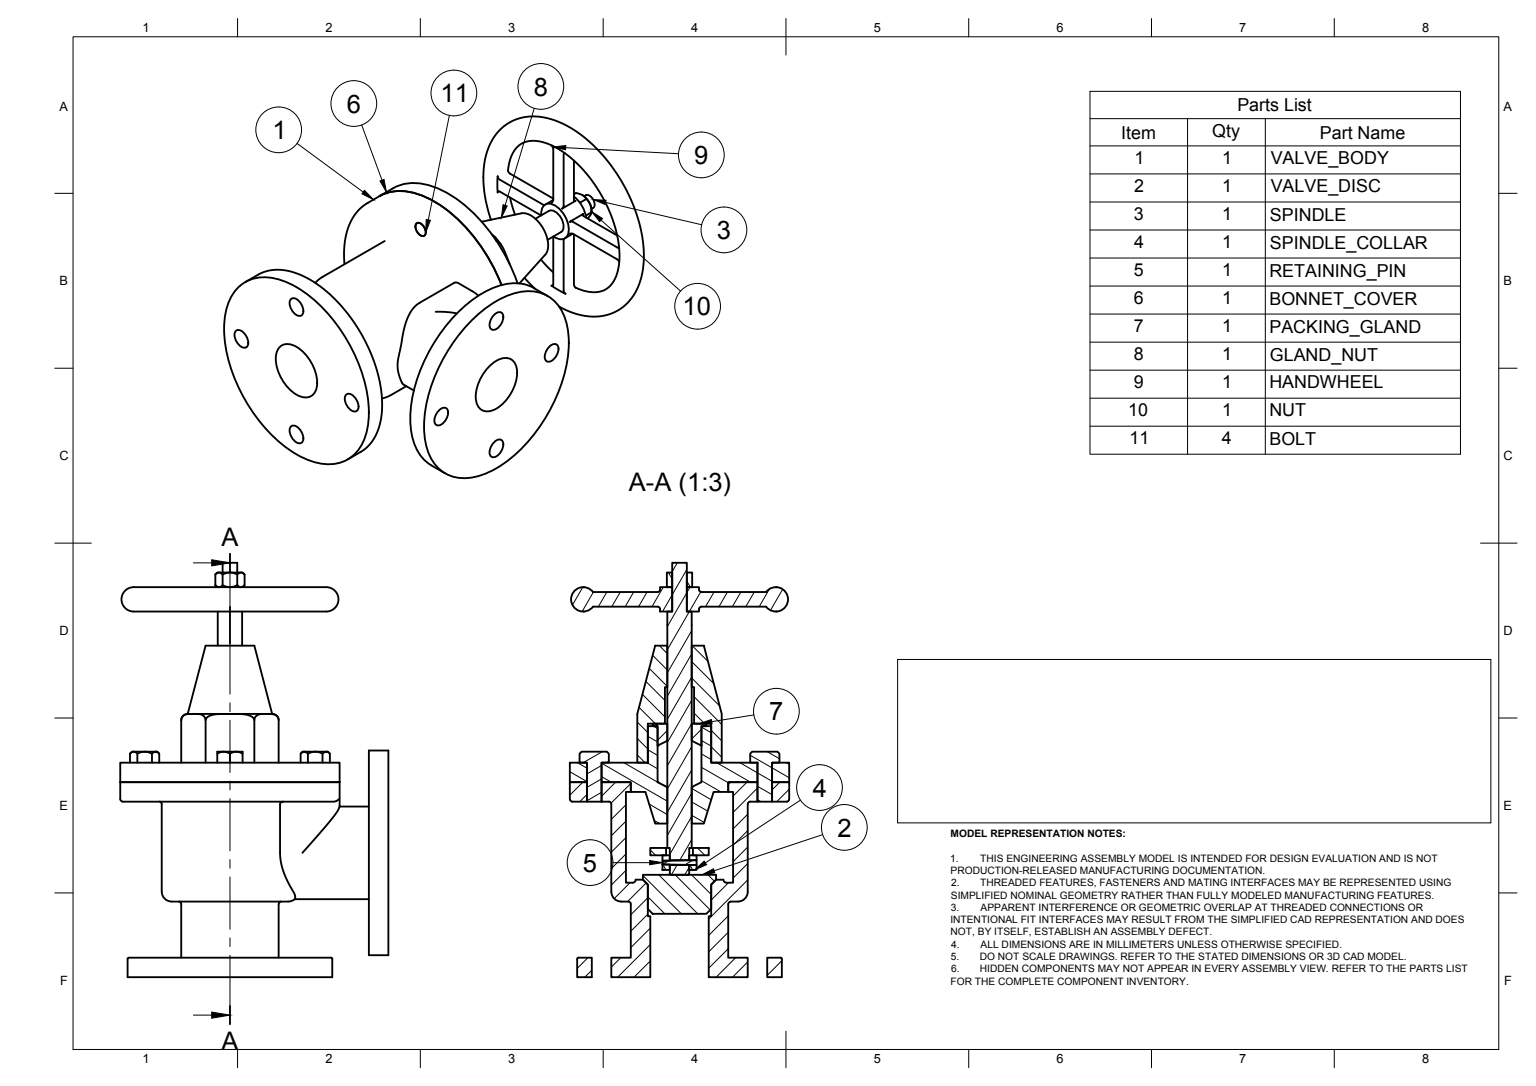
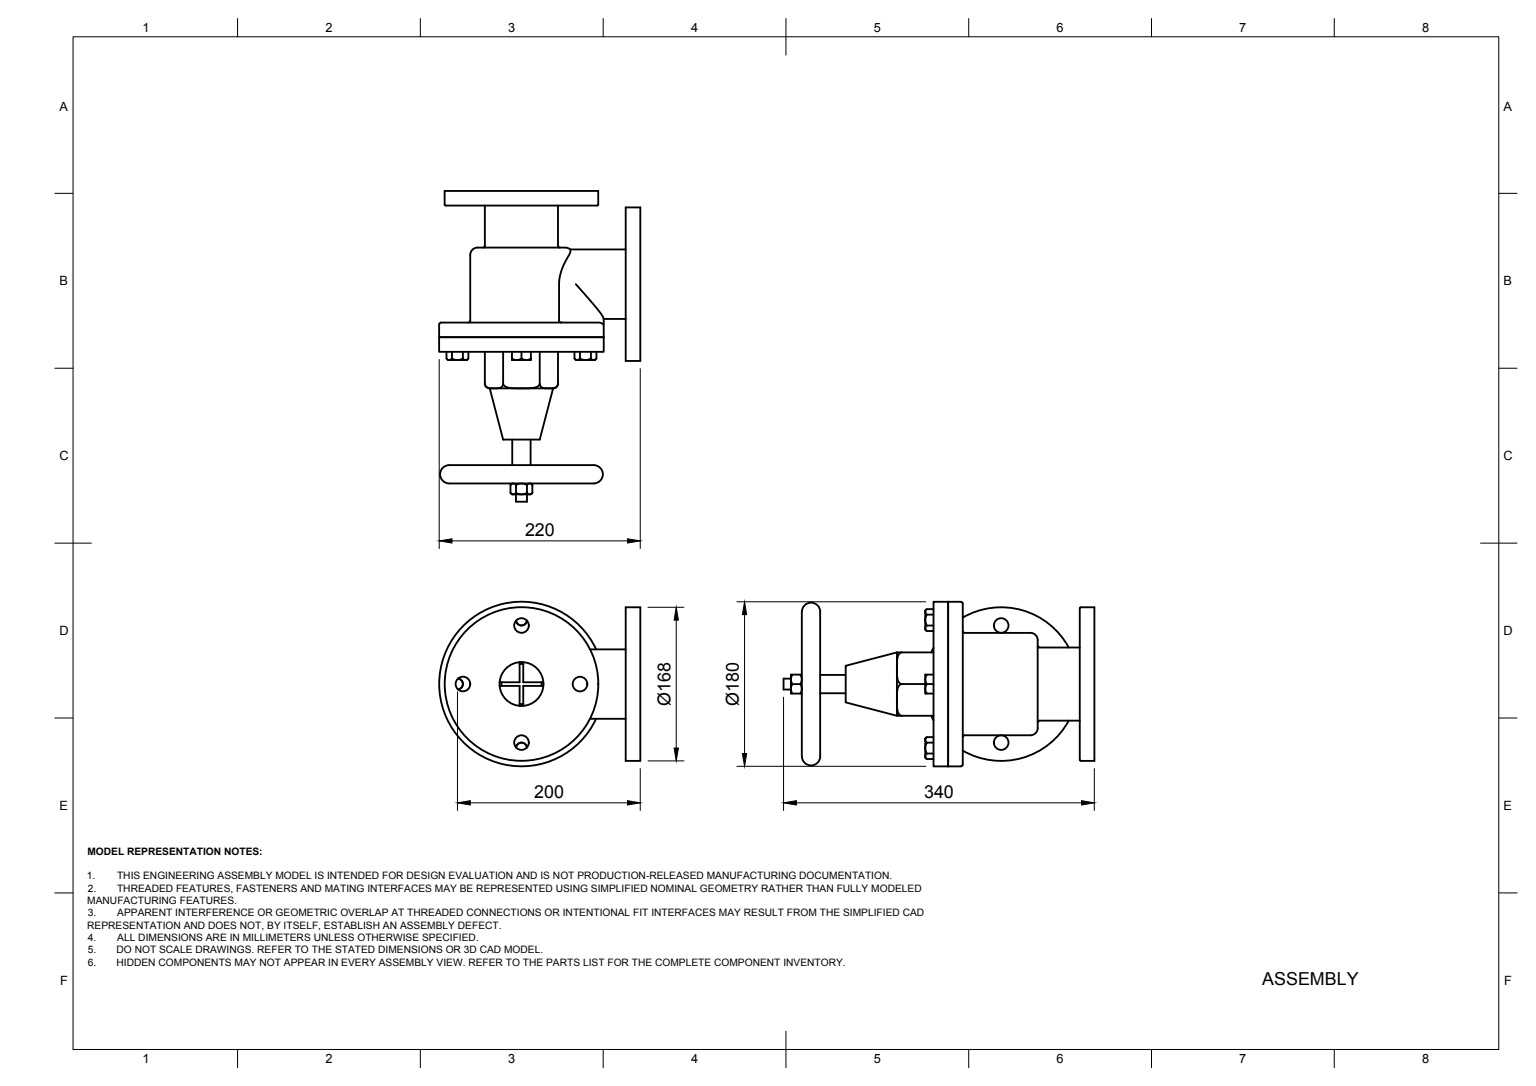
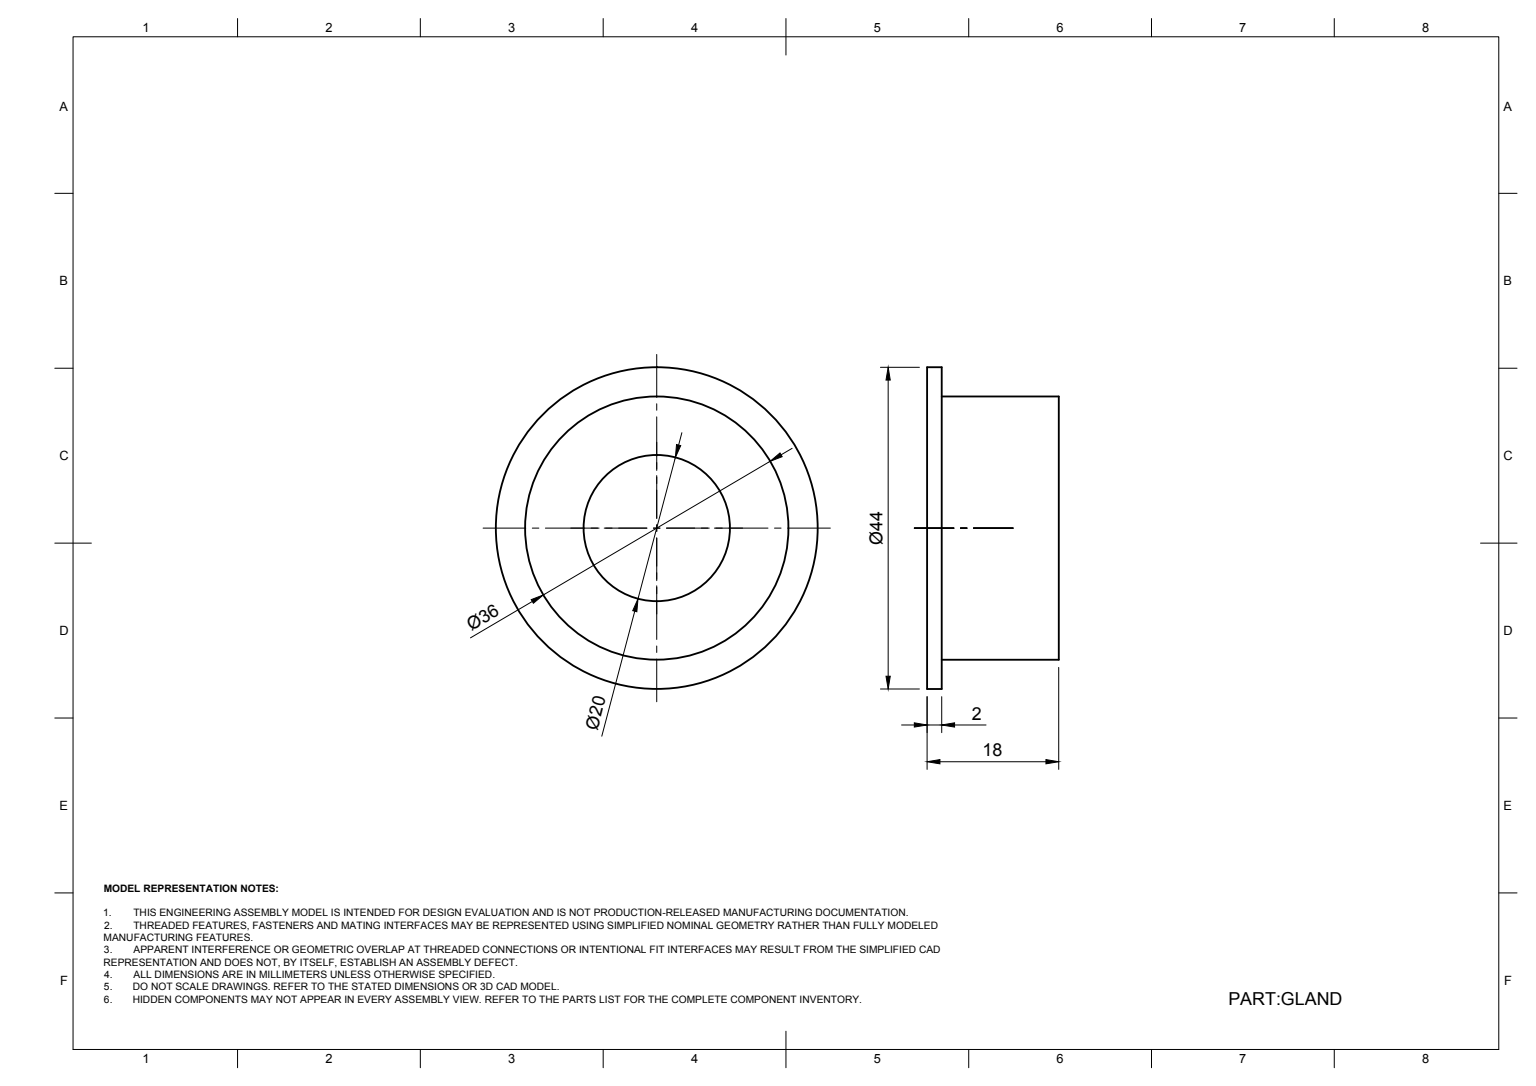
ISO-10303-21;
HEADER;
/* Generated by software containing ST-Developer
 * from STEP Tools, Inc. (www.steptools.com) 
 */

FILE_DESCRIPTION(
/* description */ (''),
/* implementation_level */ '2;1');

FILE_NAME(
/* name */ 'MAS-611',
/* time_stamp */ '2026-10-04T02:10:06-07:00',
/* author */ (''),
/* organization */ (''),
/* preprocessor_version */ 'ST-DEVELOPER v20.2',
/* originating_system */ 'Autodesk Translation Framework v15.15.0.0',
/* authorisation */ '');

FILE_SCHEMA (('AUTOMOTIVE_DESIGN { 1 0 10303 214 3 1 1 }'));
ENDSEC;

DATA;
#10=MECHANICAL_DESIGN_GEOMETRIC_PRESENTATION_REPRESENTATION('',(#141,#142,
#143,#144,#145,#146,#147,#148,#149,#150,#151),#9668);
#11=ITEM_DEFINED_TRANSFORMATION($,$,#4015,#4455);
#12=ITEM_DEFINED_TRANSFORMATION($,$,#4135,#4456);
#13=ITEM_DEFINED_TRANSFORMATION($,$,#4194,#4457);
#14=ITEM_DEFINED_TRANSFORMATION($,$,#4223,#4458);
#15=ITEM_DEFINED_TRANSFORMATION($,$,#4234,#4459);
#16=ITEM_DEFINED_TRANSFORMATION($,$,#4240,#4460);
#17=ITEM_DEFINED_TRANSFORMATION($,$,#4279,#4461);
#18=ITEM_DEFINED_TRANSFORMATION($,$,#4292,#4462);
#19=ITEM_DEFINED_TRANSFORMATION($,$,#4326,#4463);
#20=ITEM_DEFINED_TRANSFORMATION($,$,#4394,#4464);
#21=ITEM_DEFINED_TRANSFORMATION($,$,#4430,#4465);
#22=ITEM_DEFINED_TRANSFORMATION($,$,#4430,#4466);
#23=ITEM_DEFINED_TRANSFORMATION($,$,#4430,#4467);
#24=ITEM_DEFINED_TRANSFORMATION($,$,#4430,#4468);
#25=(
REPRESENTATION_RELATIONSHIP($,$,#9712,#9711)
REPRESENTATION_RELATIONSHIP_WITH_TRANSFORMATION(#11)
SHAPE_REPRESENTATION_RELATIONSHIP()
);
#26=(
REPRESENTATION_RELATIONSHIP($,$,#9713,#9711)
REPRESENTATION_RELATIONSHIP_WITH_TRANSFORMATION(#12)
SHAPE_REPRESENTATION_RELATIONSHIP()
);
#27=(
REPRESENTATION_RELATIONSHIP($,$,#9714,#9711)
REPRESENTATION_RELATIONSHIP_WITH_TRANSFORMATION(#13)
SHAPE_REPRESENTATION_RELATIONSHIP()
);
#28=(
REPRESENTATION_RELATIONSHIP($,$,#9715,#9711)
REPRESENTATION_RELATIONSHIP_WITH_TRANSFORMATION(#14)
SHAPE_REPRESENTATION_RELATIONSHIP()
);
#29=(
REPRESENTATION_RELATIONSHIP($,$,#9716,#9711)
REPRESENTATION_RELATIONSHIP_WITH_TRANSFORMATION(#15)
SHAPE_REPRESENTATION_RELATIONSHIP()
);
#30=(
REPRESENTATION_RELATIONSHIP($,$,#9717,#9711)
REPRESENTATION_RELATIONSHIP_WITH_TRANSFORMATION(#16)
SHAPE_REPRESENTATION_RELATIONSHIP()
);
#31=(
REPRESENTATION_RELATIONSHIP($,$,#9718,#9711)
REPRESENTATION_RELATIONSHIP_WITH_TRANSFORMATION(#17)
SHAPE_REPRESENTATION_RELATIONSHIP()
);
#32=(
REPRESENTATION_RELATIONSHIP($,$,#9719,#9711)
REPRESENTATION_RELATIONSHIP_WITH_TRANSFORMATION(#18)
SHAPE_REPRESENTATION_RELATIONSHIP()
);
#33=(
REPRESENTATION_RELATIONSHIP($,$,#9720,#9711)
REPRESENTATION_RELATIONSHIP_WITH_TRANSFORMATION(#19)
SHAPE_REPRESENTATION_RELATIONSHIP()
);
#34=(
REPRESENTATION_RELATIONSHIP($,$,#9721,#9711)
REPRESENTATION_RELATIONSHIP_WITH_TRANSFORMATION(#20)
SHAPE_REPRESENTATION_RELATIONSHIP()
);
#35=(
REPRESENTATION_RELATIONSHIP($,$,#9722,#9711)
REPRESENTATION_RELATIONSHIP_WITH_TRANSFORMATION(#21)
SHAPE_REPRESENTATION_RELATIONSHIP()
);
#36=(
REPRESENTATION_RELATIONSHIP($,$,#9722,#9711)
REPRESENTATION_RELATIONSHIP_WITH_TRANSFORMATION(#22)
SHAPE_REPRESENTATION_RELATIONSHIP()
);
#37=(
REPRESENTATION_RELATIONSHIP($,$,#9722,#9711)
REPRESENTATION_RELATIONSHIP_WITH_TRANSFORMATION(#23)
SHAPE_REPRESENTATION_RELATIONSHIP()
);
#38=(
REPRESENTATION_RELATIONSHIP($,$,#9722,#9711)
REPRESENTATION_RELATIONSHIP_WITH_TRANSFORMATION(#24)
SHAPE_REPRESENTATION_RELATIONSHIP()
);
#39=CONTEXT_DEPENDENT_SHAPE_REPRESENTATION(#25,#9697);
#40=CONTEXT_DEPENDENT_SHAPE_REPRESENTATION(#26,#9698);
#41=CONTEXT_DEPENDENT_SHAPE_REPRESENTATION(#27,#9699);
#42=CONTEXT_DEPENDENT_SHAPE_REPRESENTATION(#28,#9700);
#43=CONTEXT_DEPENDENT_SHAPE_REPRESENTATION(#29,#9701);
#44=CONTEXT_DEPENDENT_SHAPE_REPRESENTATION(#30,#9702);
#45=CONTEXT_DEPENDENT_SHAPE_REPRESENTATION(#31,#9703);
#46=CONTEXT_DEPENDENT_SHAPE_REPRESENTATION(#32,#9704);
#47=CONTEXT_DEPENDENT_SHAPE_REPRESENTATION(#33,#9705);
#48=CONTEXT_DEPENDENT_SHAPE_REPRESENTATION(#34,#9706);
#49=CONTEXT_DEPENDENT_SHAPE_REPRESENTATION(#35,#9707);
#50=CONTEXT_DEPENDENT_SHAPE_REPRESENTATION(#36,#9708);
#51=CONTEXT_DEPENDENT_SHAPE_REPRESENTATION(#37,#9709);
#52=CONTEXT_DEPENDENT_SHAPE_REPRESENTATION(#38,#9710);
#53=NEXT_ASSEMBLY_USAGE_OCCURRENCE('VALVE_BODY:1','VALVE_BODY:1',
'VALVE_BODY:1',#9724,#9725,'VALVE_BODY:1');
#54=NEXT_ASSEMBLY_USAGE_OCCURRENCE('VALVE_DISC:1','VALVE_DISC:1',
'VALVE_DISC:1',#9724,#9726,'VALVE_DISC:1');
#55=NEXT_ASSEMBLY_USAGE_OCCURRENCE('SPINDLE:1','SPINDLE:1','SPINDLE:1',
#9724,#9727,'SPINDLE:1');
#56=NEXT_ASSEMBLY_USAGE_OCCURRENCE('SPINDLE_COLLAR:1',
'SPINDLE_COLLAR:1','SPINDLE_COLLAR:1',#9724,#9728,'SPINDLE_COLLAR:1');
#57=NEXT_ASSEMBLY_USAGE_OCCURRENCE('RETAINING_PIN:1','RETAINING_PIN:1',
'RETAINING_PIN:1',#9724,#9729,'RETAINING_PIN:1');
#58=NEXT_ASSEMBLY_USAGE_OCCURRENCE('BONNET_COVER:1','BONNET_COVER:1',
'BONNET_COVER:1',#9724,#9730,'BONNET_COVER:1');
#59=NEXT_ASSEMBLY_USAGE_OCCURRENCE('PACKING_GLAND:1','PACKING_GLAND:1',
'PACKING_GLAND:1',#9724,#9731,'PACKING_GLAND:1');
#60=NEXT_ASSEMBLY_USAGE_OCCURRENCE('GLAND_NUT:1','GLAND_NUT:1',
'GLAND_NUT:1',#9724,#9732,'GLAND_NUT:1');
#61=NEXT_ASSEMBLY_USAGE_OCCURRENCE('HANDWHEEL:1','HANDWHEEL:1',
'HANDWHEEL:1',#9724,#9733,'HANDWHEEL:1');
#62=NEXT_ASSEMBLY_USAGE_OCCURRENCE('NUT:1','NUT:1','NUT:1',#9724,#9734,
'NUT:1');
#63=NEXT_ASSEMBLY_USAGE_OCCURRENCE('BOLT:1','BOLT:1','BOLT:1',#9724,#9735,
'BOLT:1');
#64=NEXT_ASSEMBLY_USAGE_OCCURRENCE('BOLT:2','BOLT:2','BOLT:2',#9724,#9735,
'BOLT:2');
#65=NEXT_ASSEMBLY_USAGE_OCCURRENCE('BOLT:3','BOLT:3','BOLT:3',#9724,#9735,
'BOLT:3');
#66=NEXT_ASSEMBLY_USAGE_OCCURRENCE('BOLT:4','BOLT:4','BOLT:4',#9724,#9735,
'BOLT:4');
#67=(
BOUNDED_SURFACE()
B_SPLINE_SURFACE(3,2,((#8974,#8975,#8976),(#8977,#8978,#8979),(#8980,#8981,
#8982),(#8983,#8984,#8985),(#8986,#8987,#8988),(#8989,#8990,#8991),(#8992,
#8993,#8994),(#8995,#8996,#8997),(#8998,#8999,#9000),(#9001,#9002,#9003),
(#9004,#9005,#9006),(#9007,#9008,#9009),(#9010,#9011,#9012),(#9013,#9014,
#9015),(#9016,#9017,#9018),(#9019,#9020,#9021),(#9022,#9023,#9024),(#9025,
#9026,#9027)),.UNSPECIFIED.,.F.,.F.,.F.)
B_SPLINE_SURFACE_WITH_KNOTS((4,1,1,1,1,1,1,1,1,1,1,1,1,1,1,4),(3,3),(0.0314788030428868,
0.0324522874563819,0.0334257718698771,0.0353727406968673,0.0363462251103625,
0.0373197095238576,0.0382931939373528,0.0392666783508479,0.0402401627643431,
0.0412136471778382,0.0421871315913334,0.0431606160048285,0.0441341004183236,
0.0451075848318188,0.0460810692453139,0.0470545536588091),(0.,1.),
 .UNSPECIFIED.)
GEOMETRIC_REPRESENTATION_ITEM()
RATIONAL_B_SPLINE_SURFACE(((1.,0.673965297618148,1.),(1.,0.673166296515258,
1.),(1.,0.671622878424884,1.),(1.,0.668872043360916,1.),(1.,0.6666737415125,
1.),(1.,0.665066367000124,1.),(1.,0.664191179384959,1.),(1.,0.663664801981856,
1.),(1.,0.663490402453091,1.),(1.,0.663673371681184,1.),(1.,0.664201607885415,
1.),(1.,0.66506767873011,1.),(1.,0.666279408316226,1.),(1.,0.667792932640577,
1.),(1.,0.669583017900756,1.),(1.,0.671633975311695,1.),(1.,0.673174922786531,
1.),(1.,0.673980190168732,1.)))
REPRESENTATION_ITEM('')
SURFACE()
);
#68=(
BOUNDED_SURFACE()
B_SPLINE_SURFACE(3,2,((#9028,#9029,#9030),(#9031,#9032,#9033),(#9034,#9035,
#9036),(#9037,#9038,#9039),(#9040,#9041,#9042),(#9043,#9044,#9045),(#9046,
#9047,#9048),(#9049,#9050,#9051),(#9052,#9053,#9054),(#9055,#9056,#9057),
(#9058,#9059,#9060),(#9061,#9062,#9063),(#9064,#9065,#9066),(#9067,#9068,
#9069),(#9070,#9071,#9072),(#9073,#9074,#9075),(#9076,#9077,#9078),(#9079,
#9080,#9081)),.UNSPECIFIED.,.F.,.F.,.F.)
B_SPLINE_SURFACE_WITH_KNOTS((4,1,1,1,1,1,1,1,1,1,1,1,1,1,1,4),(3,3),(0.0306904631349172,
0.0316643361466102,0.0326382091583032,0.0336120821699963,0.0345859551816893,
0.0355598281933823,0.0365337012050753,0.0375075742167683,0.0384814472284614,
0.0394553202401544,0.0404291932518474,0.0414030662635404,0.0423769392752334,
0.0433508122869265,0.0443246852986195,0.0462724313220055),(0.,1.),
 .UNSPECIFIED.)
GEOMETRIC_REPRESENTATION_ITEM()
RATIONAL_B_SPLINE_SURFACE(((1.,0.673964349039136,1.),(1.,0.673168502978567,
1.),(1.,0.671643925861953,1.),(1.,0.669562296886318,1.),(1.,0.667767007356651,
1.),(1.,0.666266776870979,1.),(1.,0.665071978074277,1.),(1.,0.664194007330874,
1.),(1.,0.663665542131989,1.),(1.,0.663490103902602,1.),(1.,0.663673710164509,
1.),(1.,0.664205908065376,1.),(1.,0.665074561266886,1.),(1.,0.666270920547672,
1.),(1.,0.667799410011383,1.),(1.,0.670197938500333,1.),(1.,0.672375755500364,
1.),(1.,0.673978916833767,1.)))
REPRESENTATION_ITEM('')
SURFACE()
);
#69=(
BOUNDED_SURFACE()
B_SPLINE_SURFACE(3,2,((#9082,#9083,#9084),(#9085,#9086,#9087),(#9088,#9089,
#9090),(#9091,#9092,#9093),(#9094,#9095,#9096),(#9097,#9098,#9099),(#9100,
#9101,#9102),(#9103,#9104,#9105),(#9106,#9107,#9108),(#9109,#9110,#9111),
(#9112,#9113,#9114),(#9115,#9116,#9117),(#9118,#9119,#9120),(#9121,#9122,
#9123),(#9124,#9125,#9126),(#9127,#9128,#9129),(#9130,#9131,#9132),(#9133,
#9134,#9135)),.UNSPECIFIED.,.F.,.F.,.F.)
B_SPLINE_SURFACE_WITH_KNOTS((4,1,1,1,1,1,1,1,1,1,1,1,1,1,1,4),(3,3),(0.0305897871911959,
0.0315636944986189,0.0325376018060419,0.0335115091134649,0.0344854164208879,
0.0354593237283109,0.0364332310357338,0.0374071383431568,0.0383810456505798,
0.0393549529580028,0.0403288602654258,0.0413027675728487,0.0422766748802717,
0.0432505821876947,0.0442244894951177,0.0461723041099637),(0.,1.),
 .UNSPECIFIED.)
GEOMETRIC_REPRESENTATION_ITEM()
RATIONAL_B_SPLINE_SURFACE(((1.,0.673964296834234,1.),(1.,0.673168609933157,
1.),(1.,0.671645019887839,1.),(1.,0.669565127304379,1.),(1.,0.667766560497273,
1.),(1.,0.666266474426915,1.),(1.,0.66507215658795,1.),(1.,0.664195156886529,
1.),(1.,0.663665573830476,1.),(1.,0.663490167959275,1.),(1.,0.663673406028792,
1.),(1.,0.664206149646574,1.),(1.,0.665075135400244,1.),(1.,0.666270395103817,
1.),(1.,0.667798233506142,1.),(1.,0.670199686629813,1.),(1.,0.672377030394903,
1.),(1.,0.673978715902987,1.)))
REPRESENTATION_ITEM('')
SURFACE()
);
#70=(
BOUNDED_SURFACE()
B_SPLINE_SURFACE(3,2,((#9136,#9137,#9138),(#9139,#9140,#9141),(#9142,#9143,
#9144),(#9145,#9146,#9147),(#9148,#9149,#9150),(#9151,#9152,#9153),(#9154,
#9155,#9156),(#9157,#9158,#9159),(#9160,#9161,#9162),(#9163,#9164,#9165),
(#9166,#9167,#9168),(#9169,#9170,#9171),(#9172,#9173,#9174),(#9175,#9176,
#9177),(#9178,#9179,#9180),(#9181,#9182,#9183),(#9184,#9185,#9186),(#9187,
#9188,#9189)),.UNSPECIFIED.,.F.,.F.,.F.)
B_SPLINE_SURFACE_WITH_KNOTS((4,1,1,1,1,1,1,1,1,1,1,1,1,1,1,4),(3,3),(0.0315789108977846,
0.0325523529389518,0.0335257949801189,0.0354726790624532,0.0364461211036204,
0.0374195631447876,0.0383930051859547,0.0393664472271219,0.040339889268289,
0.0413133313094562,0.0422867733506233,0.0432602153917905,0.0442336574329576,
0.0452070994741248,0.046180541515292,0.0471539835564591),(0.,1.),
 .UNSPECIFIED.)
GEOMETRIC_REPRESENTATION_ITEM()
RATIONAL_B_SPLINE_SURFACE(((1.,0.673965492863365,1.),(1.,0.673165826863236,
1.),(1.,0.671620469526443,1.),(1.,0.668874652098692,1.),(1.,0.666674941728974,
1.),(1.,0.665065162761098,1.),(1.,0.664191461531519,1.),(1.,0.663664604196809,
1.),(1.,0.663490522562251,1.),(1.,0.663673087023803,1.),(1.,0.664200791428412,
1.),(1.,0.665067176842279,1.),(1.,0.666279817333014,1.),(1.,0.667791010794828,
1.),(1.,0.669580698382089,1.),(1.,0.671631849583161,1.),(1.,0.673175667819509,
1.),(1.,0.673979886421463,1.)))
REPRESENTATION_ITEM('')
SURFACE()
);
#71=(
BOUNDED_SURFACE()
B_SPLINE_SURFACE(3,2,((#9190,#9191,#9192),(#9193,#9194,#9195),(#9196,#9197,
#9198),(#9199,#9200,#9201),(#9202,#9203,#9204),(#9205,#9206,#9207),(#9208,
#9209,#9210),(#9211,#9212,#9213),(#9214,#9215,#9216),(#9217,#9218,#9219),
(#9220,#9221,#9222),(#9223,#9224,#9225),(#9226,#9227,#9228),(#9229,#9230,
#9231),(#9232,#9233,#9234),(#9235,#9236,#9237)),.UNSPECIFIED.,.F.,.F.,.F.)
B_SPLINE_SURFACE_WITH_KNOTS((4,1,1,1,1,1,1,1,1,1,1,1,1,4),(3,3),(0.03215789731342,
0.0331313751868945,0.034104853060369,0.0350783309338435,0.0360518088073179,
0.0370252866807924,0.0379987645542669,0.0389722424277414,0.0399457203012159,
0.0418926760481649,0.0438396317951138,0.0457865875420628,0.0467600654155373,
0.0477335432890118),(-8.08454907084105E-6,1.),.UNSPECIFIED.)
GEOMETRIC_REPRESENTATION_ITEM()
RATIONAL_B_SPLINE_SURFACE(((1.00000527170182,0.673964387359616,1.),(1.00000528471687,
0.673159453411099,1.),(1.00000530961685,0.671619480347489,1.),(1.00000534275063,
0.669570276226346,1.),(1.00000537166522,0.66778201413489,1.),(1.00000539609675,
0.666271012581043,1.),(1.00000541568478,0.665059564372101,1.),(1.00000542974255,
0.664190142086893,1.),(1.000005438313,0.663660090710924,1.),(1.00000544199604,
0.663432308407853,1.),(1.00000543253772,0.664017270646154,1.),(1.00000539844928,
0.666125517336438,1.),(1.00000535391695,0.668879680311451,1.),(1.00000530941503,
0.671631962440139,1.),(1.00000528444356,0.673176357213759,1.),(1.00000527151599,
0.673975880021096,1.)))
REPRESENTATION_ITEM('')
SURFACE()
);
#72=(
BOUNDED_SURFACE()
B_SPLINE_SURFACE(3,2,((#9238,#9239,#9240),(#9241,#9242,#9243),(#9244,#9245,
#9246),(#9247,#9248,#9249),(#9250,#9251,#9252),(#9253,#9254,#9255),(#9256,
#9257,#9258),(#9259,#9260,#9261),(#9262,#9263,#9264),(#9265,#9266,#9267),
(#9268,#9269,#9270),(#9271,#9272,#9273),(#9274,#9275,#9276),(#9277,#9278,
#9279),(#9280,#9281,#9282),(#9283,#9284,#9285)),.UNSPECIFIED.,.F.,.F.,.F.)
B_SPLINE_SURFACE_WITH_KNOTS((4,1,1,1,1,1,1,1,1,1,1,1,1,4),(3,3),(0.0300049518513901,
0.031953018177045,0.0329270513398724,0.0339010845026998,0.0348751176655272,
0.0358491508283546,0.036823183991182,0.0377972171540094,0.0387712503168368,
0.0397452834796642,0.041693349805319,0.0426673829681464,0.0436414161309738,
0.0455894824566286),(0.,1.),.UNSPECIFIED.)
GEOMETRIC_REPRESENTATION_ITEM()
RATIONAL_B_SPLINE_SURFACE(((1.,0.673964297815332,1.),(1.,0.672372618458235,
1.),(1.,0.670191181394266,1.),(1.,0.667767841290405,1.),(1.,0.666265347639804,
1.),(1.,0.665072121147338,1.),(1.,0.664201207028703,1.),(1.,0.663666605647771,
1.),(1.,0.663490715236844,1.),(1.,0.663670119784287,1.),(1.,0.664385152559804,
1.),(1.,0.665767066134064,1.),(1.,0.66778345083312,1.),(1.,0.670206332337341,
1.),(1.,0.672382580991143,1.),(1.,0.673977852527306,1.)))
REPRESENTATION_ITEM('')
SURFACE()
);
#73=(
BOUNDED_SURFACE()
B_SPLINE_SURFACE(3,2,((#9286,#9287,#9288),(#9289,#9290,#9291),(#9292,#9293,
#9294),(#9295,#9296,#9297),(#9298,#9299,#9300),(#9301,#9302,#9303),(#9304,
#9305,#9306),(#9307,#9308,#9309),(#9310,#9311,#9312),(#9313,#9314,#9315),
(#9316,#9317,#9318),(#9319,#9320,#9321),(#9322,#9323,#9324),(#9325,#9326,
#9327),(#9328,#9329,#9330),(#9331,#9332,#9333),(#9334,#9335,#9336),(#9337,
#9338,#9339),(#9340,#9341,#9342)),.UNSPECIFIED.,.F.,.F.,.F.)
B_SPLINE_SURFACE_WITH_KNOTS((4,1,1,1,1,1,1,1,1,1,1,1,1,1,1,1,4),(3,3),(0.0317649381765832,
0.0327383392942574,0.0337117404119316,0.0346851415296058,0.03565854264728,
0.0366319437649542,0.0376053448826284,0.0385787460003026,0.0395521471179768,
0.040525548235651,0.0414989493533253,0.0424723504709995,0.0434457515886737,
0.0444191527063479,0.0453925538240221,0.0463659549416963,0.0473393560593705),
(0.,1.),.UNSPECIFIED.)
GEOMETRIC_REPRESENTATION_ITEM()
RATIONAL_B_SPLINE_SURFACE(((1.,0.673965909365134,1.),(1.,0.673164818236142,
1.),(1.,0.671618061862569,1.),(1.,0.669564320284071,1.),(1.,0.66777759511695,
1.),(1.,0.666273471258361,1.),(1.,0.665063410818969,1.),(1.,0.664191967652661,
1.),(1.,0.663664156821065,1.),(1.,0.663490769293391,1.),(1.,0.663672536496092,
1.),(1.,0.664199292987571,1.),(1.,0.665067031441957,1.),(1.,0.666280071948857,
1.),(1.,0.66778774864528,1.),(1.,0.669576760671401,1.),(1.,0.671629936935393,
1.),(1.,0.673176919539912,1.),(1.,0.673979374441674,1.)))
REPRESENTATION_ITEM('')
SURFACE()
);
#74=(
BOUNDED_SURFACE()
B_SPLINE_SURFACE(3,2,((#9343,#9344,#9345),(#9346,#9347,#9348),(#9349,#9350,
#9351),(#9352,#9353,#9354),(#9355,#9356,#9357),(#9358,#9359,#9360),(#9361,
#9362,#9363),(#9364,#9365,#9366),(#9367,#9368,#9369),(#9370,#9371,#9372),
(#9373,#9374,#9375),(#9376,#9377,#9378),(#9379,#9380,#9381),(#9382,#9383,
#9384),(#9385,#9386,#9387),(#9388,#9389,#9390),(#9391,#9392,#9393)),
 .UNSPECIFIED.,.F.,.F.,.F.)
B_SPLINE_SURFACE_WITH_KNOTS((4,1,1,1,1,1,1,1,1,1,1,1,1,1,4),(3,3),(0.0304023584176636,
0.0313763197495467,0.0323502810814299,0.0333242424133131,0.0342982037451962,
0.0352721650770794,0.0362461264089626,0.0372200877408457,0.0381940490727289,
0.0391680104046121,0.0401419717364953,0.0420898944002616,0.0430638557321448,
0.0440378170640279,0.0459857397277943),(0.,1.),.UNSPECIFIED.)
GEOMETRIC_REPRESENTATION_ITEM()
RATIONAL_B_SPLINE_SURFACE(((1.,0.673964240667089,1.),(1.,0.673168704865034,
1.),(1.,0.671646043506943,1.),(1.,0.669571927360062,1.),(1.,0.667765968900773,
1.),(1.,0.666266091842261,1.),(1.,0.665072243840693,1.),(1.,0.664197515743925,
1.),(1.,0.663665655019745,1.),(1.,0.663490373557035,1.),(1.,0.663672476132646,
1.),(1.,0.664385168150455,1.),(1.,0.665762507320331,1.),(1.,0.667794613454947,
1.),(1.,0.670202685638588,1.),(1.,0.672379152055614,1.),(1.,0.6739783830491,
1.)))
REPRESENTATION_ITEM('')
SURFACE()
);
#75=(
BOUNDED_CURVE()
B_SPLINE_CURVE(2,(#6291,#6292,#6293),.UNSPECIFIED.,.F.,.F.)
B_SPLINE_CURVE_WITH_KNOTS((3,3),(-0.968089558975317,-0.208236182755166),
 .UNSPECIFIED.)
CURVE()
GEOMETRIC_REPRESENTATION_ITEM()
RATIONAL_B_SPLINE_CURVE((1.03202593839996,1.02394290093172,1.00881846372195))
REPRESENTATION_ITEM('')
);
#76=(
BOUNDED_CURVE()
B_SPLINE_CURVE(2,(#6302,#6303,#6304),.UNSPECIFIED.,.F.,.F.)
B_SPLINE_CURVE_WITH_KNOTS((3,3),(-3.47246065490362,-2.71260727868867),
 .UNSPECIFIED.)
CURVE()
GEOMETRIC_REPRESENTATION_ITEM()
RATIONAL_B_SPLINE_CURVE((1.00881846372215,1.02394290093178,1.03202593839996))
REPRESENTATION_ITEM('')
);
#77=(
BOUNDED_CURVE()
B_SPLINE_CURVE(2,(#6312,#6313,#6314),.UNSPECIFIED.,.F.,.F.)
B_SPLINE_CURVE_WITH_KNOTS((3,3),(-3.47246065490362,-2.71260727868867),
 .UNSPECIFIED.)
CURVE()
GEOMETRIC_REPRESENTATION_ITEM()
RATIONAL_B_SPLINE_CURVE((1.00881846372215,1.02394290093178,1.03202593839996))
REPRESENTATION_ITEM('')
);
#78=(
BOUNDED_CURVE()
B_SPLINE_CURVE(2,(#6321,#6322,#6323),.UNSPECIFIED.,.F.,.F.)
B_SPLINE_CURVE_WITH_KNOTS((3,3),(-0.968089558975317,-0.208236182755166),
 .UNSPECIFIED.)
CURVE()
GEOMETRIC_REPRESENTATION_ITEM()
RATIONAL_B_SPLINE_CURVE((1.03202593839996,1.02394290093172,1.00881846372195))
REPRESENTATION_ITEM('')
);
#79=(
BOUNDED_CURVE()
B_SPLINE_CURVE(2,(#6399,#6400,#6401),.UNSPECIFIED.,.F.,.F.)
B_SPLINE_CURVE_WITH_KNOTS((3,3),(-3.47246065490413,-2.71260727868925),
 .UNSPECIFIED.)
CURVE()
GEOMETRIC_REPRESENTATION_ITEM()
RATIONAL_B_SPLINE_CURVE((1.00881846372252,1.0239429009328,1.03202593840134))
REPRESENTATION_ITEM('')
);
#80=(
BOUNDED_CURVE()
B_SPLINE_CURVE(2,(#6406,#6407,#6408),.UNSPECIFIED.,.F.,.F.)
B_SPLINE_CURVE_WITH_KNOTS((3,3),(-0.968089559028266,-0.20823618276597),
 .UNSPECIFIED.)
CURVE()
GEOMETRIC_REPRESENTATION_ITEM()
RATIONAL_B_SPLINE_CURVE((1.03202593842995,1.02394290095447,1.00881846373032))
REPRESENTATION_ITEM('')
);
#81=(
BOUNDED_CURVE()
B_SPLINE_CURVE(2,(#6413,#6414,#6415),.UNSPECIFIED.,.F.,.F.)
B_SPLINE_CURVE_WITH_KNOTS((3,3),(-3.47246065490413,-2.71260727868925),
 .UNSPECIFIED.)
CURVE()
GEOMETRIC_REPRESENTATION_ITEM()
RATIONAL_B_SPLINE_CURVE((1.00881846372251,1.0239429009328,1.03202593840134))
REPRESENTATION_ITEM('')
);
#82=(
BOUNDED_CURVE()
B_SPLINE_CURVE(2,(#6420,#6421,#6422),.UNSPECIFIED.,.F.,.F.)
B_SPLINE_CURVE_WITH_KNOTS((3,3),(-0.968089559028514,-0.208236182766157),
 .UNSPECIFIED.)
CURVE()
GEOMETRIC_REPRESENTATION_ITEM()
RATIONAL_B_SPLINE_CURVE((1.03202593842948,1.02394290095412,1.0088184637302))
REPRESENTATION_ITEM('')
);
#83=(
BOUNDED_CURVE()
B_SPLINE_CURVE(2,(#9398,#9399,#9400),.UNSPECIFIED.,.F.,.F.)
B_SPLINE_CURVE_WITH_KNOTS((3,3),(1.40089977676118,2.46618168478736),
 .UNSPECIFIED.)
CURVE()
GEOMETRIC_REPRESENTATION_ITEM()
RATIONAL_B_SPLINE_CURVE((1.50876305611317,1.62546628464682,1.62546628464682))
REPRESENTATION_ITEM('')
);
#84=(
BOUNDED_CURVE()
B_SPLINE_CURVE(2,(#9404,#9405,#9406),.UNSPECIFIED.,.F.,.F.)
B_SPLINE_CURVE_WITH_KNOTS((3,3),(2.46617097132528,3.53145008162195),
 .UNSPECIFIED.)
CURVE()
GEOMETRIC_REPRESENTATION_ITEM()
RATIONAL_B_SPLINE_CURVE((1.6254627916221,1.6254627916221,1.50875981387633))
REPRESENTATION_ITEM('')
);
#85=(
BOUNDED_CURVE()
B_SPLINE_CURVE(2,(#9408,#9409,#9410),.UNSPECIFIED.,.F.,.F.)
B_SPLINE_CURVE_WITH_KNOTS((3,3),(1.40089186102861,2.46617097132528),
 .UNSPECIFIED.)
CURVE()
GEOMETRIC_REPRESENTATION_ITEM()
RATIONAL_B_SPLINE_CURVE((1.50875981387633,1.6254627916221,1.6254627916221))
REPRESENTATION_ITEM('')
);
#86=(
BOUNDED_CURVE()
B_SPLINE_CURVE(2,(#9413,#9414,#9415),.UNSPECIFIED.,.F.,.F.)
B_SPLINE_CURVE_WITH_KNOTS((3,3),(2.46617097132528,3.5314500816219),
 .UNSPECIFIED.)
CURVE()
GEOMETRIC_REPRESENTATION_ITEM()
RATIONAL_B_SPLINE_CURVE((1.6254627916221,1.6254627916221,1.50875981387634))
REPRESENTATION_ITEM('')
);
#87=(
BOUNDED_CURVE()
B_SPLINE_CURVE(2,(#9419,#9420,#9421),.UNSPECIFIED.,.F.,.F.)
B_SPLINE_CURVE_WITH_KNOTS((3,3),(1.40089977676118,2.46618168478736),
 .UNSPECIFIED.)
CURVE()
GEOMETRIC_REPRESENTATION_ITEM()
RATIONAL_B_SPLINE_CURVE((1.50876305611317,1.62546628464682,1.62546628464682))
REPRESENTATION_ITEM('')
);
#88=(
BOUNDED_CURVE()
B_SPLINE_CURVE(2,(#9425,#9426,#9427),.UNSPECIFIED.,.F.,.F.)
B_SPLINE_CURVE_WITH_KNOTS((3,3),(2.46617097132528,3.53145008162194),
 .UNSPECIFIED.)
CURVE()
GEOMETRIC_REPRESENTATION_ITEM()
RATIONAL_B_SPLINE_CURVE((1.6254627916221,1.6254627916221,1.50875981387633))
REPRESENTATION_ITEM('')
);
#89=(
BOUNDED_CURVE()
B_SPLINE_CURVE(2,(#9428,#9429,#9430),.UNSPECIFIED.,.F.,.F.)
B_SPLINE_CURVE_WITH_KNOTS((3,3),(1.40089186102861,2.46617097132528),
 .UNSPECIFIED.)
CURVE()
GEOMETRIC_REPRESENTATION_ITEM()
RATIONAL_B_SPLINE_CURVE((1.50875981387633,1.6254627916221,1.6254627916221))
REPRESENTATION_ITEM('')
);
#90=(
BOUNDED_CURVE()
B_SPLINE_CURVE(2,(#9431,#9432,#9433),.UNSPECIFIED.,.F.,.F.)
B_SPLINE_CURVE_WITH_KNOTS((3,3),(2.46617097132528,3.53145008162195),
 .UNSPECIFIED.)
CURVE()
GEOMETRIC_REPRESENTATION_ITEM()
RATIONAL_B_SPLINE_CURVE((1.6254627916221,1.6254627916221,1.50875981387633))
REPRESENTATION_ITEM('')
);
#91=(
BOUNDED_CURVE()
B_SPLINE_CURVE(2,(#9437,#9438,#9439),.UNSPECIFIED.,.F.,.F.)
B_SPLINE_CURVE_WITH_KNOTS((3,3),(1.4008995977322,2.46618144248253),
 .UNSPECIFIED.)
CURVE()
GEOMETRIC_REPRESENTATION_ITEM()
RATIONAL_B_SPLINE_CURVE((1.50876298278395,1.62546620564557,1.62546620564557))
REPRESENTATION_ITEM('')
);
#92=(
BOUNDED_CURVE()
B_SPLINE_CURVE(2,(#9443,#9444,#9445),.UNSPECIFIED.,.F.,.F.)
B_SPLINE_CURVE_WITH_KNOTS((3,3),(2.46618137387007,3.53146320070284),
 .UNSPECIFIED.)
CURVE()
GEOMETRIC_REPRESENTATION_ITEM()
RATIONAL_B_SPLINE_CURVE((1.62546618327512,1.62546618327512,1.50876296201962))
REPRESENTATION_ITEM('')
);
#93=(
BOUNDED_CURVE()
B_SPLINE_CURVE(2,(#9446,#9447,#9448),.UNSPECIFIED.,.F.,.F.)
B_SPLINE_CURVE_WITH_KNOTS((3,3),(1.4008995470373,2.46618137387007),
 .UNSPECIFIED.)
CURVE()
GEOMETRIC_REPRESENTATION_ITEM()
RATIONAL_B_SPLINE_CURVE((1.50876296201962,1.62546618327511,1.62546618327511))
REPRESENTATION_ITEM('')
);
#94=(
BOUNDED_CURVE()
B_SPLINE_CURVE(2,(#9449,#9450,#9451),.UNSPECIFIED.,.F.,.F.)
B_SPLINE_CURVE_WITH_KNOTS((3,3),(2.46617097132528,3.53145008162195),
 .UNSPECIFIED.)
CURVE()
GEOMETRIC_REPRESENTATION_ITEM()
RATIONAL_B_SPLINE_CURVE((1.6254627916221,1.6254627916221,1.50875981387633))
REPRESENTATION_ITEM('')
);
#95=(
BOUNDED_CURVE()
B_SPLINE_CURVE(2,(#9455,#9456,#9457),.UNSPECIFIED.,.F.,.F.)
B_SPLINE_CURVE_WITH_KNOTS((3,3),(1.40089977676118,2.46618168478736),
 .UNSPECIFIED.)
CURVE()
GEOMETRIC_REPRESENTATION_ITEM()
RATIONAL_B_SPLINE_CURVE((1.50876305611317,1.62546628464682,1.62546628464682))
REPRESENTATION_ITEM('')
);
#96=(
BOUNDED_CURVE()
B_SPLINE_CURVE(2,(#9461,#9462,#9463),.UNSPECIFIED.,.F.,.F.)
B_SPLINE_CURVE_WITH_KNOTS((3,3),(2.46617097132528,3.53145008162195),
 .UNSPECIFIED.)
CURVE()
GEOMETRIC_REPRESENTATION_ITEM()
RATIONAL_B_SPLINE_CURVE((1.6254627916221,1.6254627916221,1.50875981387633))
REPRESENTATION_ITEM('')
);
#97=(
BOUNDED_CURVE()
B_SPLINE_CURVE(2,(#9464,#9465,#9466),.UNSPECIFIED.,.F.,.F.)
B_SPLINE_CURVE_WITH_KNOTS((3,3),(1.40089186102861,2.46617097132528),
 .UNSPECIFIED.)
CURVE()
GEOMETRIC_REPRESENTATION_ITEM()
RATIONAL_B_SPLINE_CURVE((1.50875981387633,1.6254627916221,1.6254627916221))
REPRESENTATION_ITEM('')
);
#98=(
BOUNDED_CURVE()
B_SPLINE_CURVE(2,(#9467,#9468,#9469),.UNSPECIFIED.,.F.,.F.)
B_SPLINE_CURVE_WITH_KNOTS((3,3),(2.46617097132528,3.53145008162195),
 .UNSPECIFIED.)
CURVE()
GEOMETRIC_REPRESENTATION_ITEM()
RATIONAL_B_SPLINE_CURVE((1.62546279162209,1.62546279162209,1.50875981387633))
REPRESENTATION_ITEM('')
);
#99=(
BOUNDED_CURVE()
B_SPLINE_CURVE(2,(#9473,#9474,#9475),.UNSPECIFIED.,.F.,.F.)
B_SPLINE_CURVE_WITH_KNOTS((3,3),(1.40089977676118,2.46618168478736),
 .UNSPECIFIED.)
CURVE()
GEOMETRIC_REPRESENTATION_ITEM()
RATIONAL_B_SPLINE_CURVE((1.50876305611317,1.62546628464682,1.62546628464682))
REPRESENTATION_ITEM('')
);
#100=(
BOUNDED_CURVE()
B_SPLINE_CURVE(2,(#9479,#9480,#9481),.UNSPECIFIED.,.F.,.F.)
B_SPLINE_CURVE_WITH_KNOTS((3,3),(2.46617097132528,3.53145008162194),
 .UNSPECIFIED.)
CURVE()
GEOMETRIC_REPRESENTATION_ITEM()
RATIONAL_B_SPLINE_CURVE((1.6254627916221,1.6254627916221,1.50875981387634))
REPRESENTATION_ITEM('')
);
#101=(
BOUNDED_CURVE()
B_SPLINE_CURVE(2,(#9482,#9483,#9484),.UNSPECIFIED.,.F.,.F.)
B_SPLINE_CURVE_WITH_KNOTS((3,3),(1.40089186102861,2.46617097132528),
 .UNSPECIFIED.)
CURVE()
GEOMETRIC_REPRESENTATION_ITEM()
RATIONAL_B_SPLINE_CURVE((1.50875981387633,1.6254627916221,1.6254627916221))
REPRESENTATION_ITEM('')
);
#102=(
BOUNDED_CURVE()
B_SPLINE_CURVE(2,(#9485,#9486,#9487),.UNSPECIFIED.,.F.,.F.)
B_SPLINE_CURVE_WITH_KNOTS((3,3),(2.46617097132529,3.53145008162195),
 .UNSPECIFIED.)
CURVE()
GEOMETRIC_REPRESENTATION_ITEM()
RATIONAL_B_SPLINE_CURVE((1.6254627916221,1.6254627916221,1.50875981387633))
REPRESENTATION_ITEM('')
);
#103=(
BOUNDED_CURVE()
B_SPLINE_CURVE(2,(#9490,#9491,#9492),.UNSPECIFIED.,.F.,.F.)
B_SPLINE_CURVE_WITH_KNOTS((3,3),(1.4008995977321,2.46618144248253),
 .UNSPECIFIED.)
CURVE()
GEOMETRIC_REPRESENTATION_ITEM()
RATIONAL_B_SPLINE_CURVE((1.50876298278393,1.62546620564557,1.62546620564557))
REPRESENTATION_ITEM('')
);
#104=(
BOUNDED_CURVE()
B_SPLINE_CURVE(2,(#9494,#9495,#9496),.UNSPECIFIED.,.F.,.F.)
B_SPLINE_CURVE_WITH_KNOTS((3,3),(2.46618137387007,3.53146320070284),
 .UNSPECIFIED.)
CURVE()
GEOMETRIC_REPRESENTATION_ITEM()
RATIONAL_B_SPLINE_CURVE((1.62546618327512,1.62546618327512,1.50876296201962))
REPRESENTATION_ITEM('')
);
#105=(
BOUNDED_CURVE()
B_SPLINE_CURVE(2,(#9497,#9498,#9499),.UNSPECIFIED.,.F.,.F.)
B_SPLINE_CURVE_WITH_KNOTS((3,3),(1.4008995470373,2.46618137387007),
 .UNSPECIFIED.)
CURVE()
GEOMETRIC_REPRESENTATION_ITEM()
RATIONAL_B_SPLINE_CURVE((1.50876296201962,1.62546618327511,1.62546618327511))
REPRESENTATION_ITEM('')
);
#106=(
BOUNDED_CURVE()
B_SPLINE_CURVE(2,(#9500,#9501,#9502),.UNSPECIFIED.,.F.,.F.)
B_SPLINE_CURVE_WITH_KNOTS((3,3),(2.46617097132528,3.53145008162195),
 .UNSPECIFIED.)
CURVE()
GEOMETRIC_REPRESENTATION_ITEM()
RATIONAL_B_SPLINE_CURVE((1.6254627916221,1.6254627916221,1.50875981387633))
REPRESENTATION_ITEM('')
);
#107=(
BOUNDED_CURVE()
B_SPLINE_CURVE(2,(#9539,#9540,#9541),.UNSPECIFIED.,.F.,.F.)
B_SPLINE_CURVE_WITH_KNOTS((3,3),(1.0700801839918,2.01951998481884),
 .UNSPECIFIED.)
CURVE()
GEOMETRIC_REPRESENTATION_ITEM()
RATIONAL_B_SPLINE_CURVE((1.37478521766072,1.48112522432469,1.48112522432469))
REPRESENTATION_ITEM('')
);
#108=(
BOUNDED_CURVE()
B_SPLINE_CURVE(2,(#9548,#9549,#9550),.UNSPECIFIED.,.F.,.F.)
B_SPLINE_CURVE_WITH_KNOTS((3,3),(2.01951998481884,2.96895978564587),
 .UNSPECIFIED.)
CURVE()
GEOMETRIC_REPRESENTATION_ITEM()
RATIONAL_B_SPLINE_CURVE((1.48112522432469,1.48112522432469,1.37478521766072))
REPRESENTATION_ITEM('')
);
#109=(
BOUNDED_CURVE()
B_SPLINE_CURVE(2,(#9553,#9554,#9555),.UNSPECIFIED.,.F.,.F.)
B_SPLINE_CURVE_WITH_KNOTS((3,3),(1.0700801839918,2.01951998481884),
 .UNSPECIFIED.)
CURVE()
GEOMETRIC_REPRESENTATION_ITEM()
RATIONAL_B_SPLINE_CURVE((1.37478521766072,1.48112522432469,1.48112522432469))
REPRESENTATION_ITEM('')
);
#110=(
BOUNDED_CURVE()
B_SPLINE_CURVE(2,(#9560,#9561,#9562),.UNSPECIFIED.,.F.,.F.)
B_SPLINE_CURVE_WITH_KNOTS((3,3),(2.01951998481884,2.96895978564588),
 .UNSPECIFIED.)
CURVE()
GEOMETRIC_REPRESENTATION_ITEM()
RATIONAL_B_SPLINE_CURVE((1.48112522432469,1.48112522432469,1.37478521766072))
REPRESENTATION_ITEM('')
);
#111=(
BOUNDED_CURVE()
B_SPLINE_CURVE(2,(#9565,#9566,#9567),.UNSPECIFIED.,.F.,.F.)
B_SPLINE_CURVE_WITH_KNOTS((3,3),(1.0700801839918,2.01951998481883),
 .UNSPECIFIED.)
CURVE()
GEOMETRIC_REPRESENTATION_ITEM()
RATIONAL_B_SPLINE_CURVE((1.37478521766072,1.48112522432469,1.48112522432469))
REPRESENTATION_ITEM('')
);
#112=(
BOUNDED_CURVE()
B_SPLINE_CURVE(2,(#9572,#9573,#9574),.UNSPECIFIED.,.F.,.F.)
B_SPLINE_CURVE_WITH_KNOTS((3,3),(2.01951998481883,2.96895978564588),
 .UNSPECIFIED.)
CURVE()
GEOMETRIC_REPRESENTATION_ITEM()
RATIONAL_B_SPLINE_CURVE((1.48112522432469,1.48112522432469,1.37478521766072))
REPRESENTATION_ITEM('')
);
#113=(
BOUNDED_CURVE()
B_SPLINE_CURVE(2,(#9577,#9578,#9579),.UNSPECIFIED.,.F.,.F.)
B_SPLINE_CURVE_WITH_KNOTS((3,3),(1.0700801839918,2.01951998481884),
 .UNSPECIFIED.)
CURVE()
GEOMETRIC_REPRESENTATION_ITEM()
RATIONAL_B_SPLINE_CURVE((1.37478521766072,1.48112522432469,1.48112522432469))
REPRESENTATION_ITEM('')
);
#114=(
BOUNDED_CURVE()
B_SPLINE_CURVE(2,(#9584,#9585,#9586),.UNSPECIFIED.,.F.,.F.)
B_SPLINE_CURVE_WITH_KNOTS((3,3),(2.01951998481884,2.96895978564587),
 .UNSPECIFIED.)
CURVE()
GEOMETRIC_REPRESENTATION_ITEM()
RATIONAL_B_SPLINE_CURVE((1.48112522432469,1.48112522432469,1.37478521766072))
REPRESENTATION_ITEM('')
);
#115=(
BOUNDED_CURVE()
B_SPLINE_CURVE(2,(#9589,#9590,#9591),.UNSPECIFIED.,.F.,.F.)
B_SPLINE_CURVE_WITH_KNOTS((3,3),(1.0700801839918,2.01951998481884),
 .UNSPECIFIED.)
CURVE()
GEOMETRIC_REPRESENTATION_ITEM()
RATIONAL_B_SPLINE_CURVE((1.37478521766072,1.48112522432469,1.48112522432469))
REPRESENTATION_ITEM('')
);
#116=(
BOUNDED_CURVE()
B_SPLINE_CURVE(2,(#9596,#9597,#9598),.UNSPECIFIED.,.F.,.F.)
B_SPLINE_CURVE_WITH_KNOTS((3,3),(2.01951998481884,2.96895978564587),
 .UNSPECIFIED.)
CURVE()
GEOMETRIC_REPRESENTATION_ITEM()
RATIONAL_B_SPLINE_CURVE((1.48112522432469,1.48112522432469,1.37478521766072))
REPRESENTATION_ITEM('')
);
#117=(
BOUNDED_CURVE()
B_SPLINE_CURVE(2,(#9601,#9602,#9603),.UNSPECIFIED.,.F.,.F.)
B_SPLINE_CURVE_WITH_KNOTS((3,3),(1.0700801839918,2.01951998481884),
 .UNSPECIFIED.)
CURVE()
GEOMETRIC_REPRESENTATION_ITEM()
RATIONAL_B_SPLINE_CURVE((1.37478521766072,1.48112522432469,1.48112522432469))
REPRESENTATION_ITEM('')
);
#118=(
BOUNDED_CURVE()
B_SPLINE_CURVE(2,(#9605,#9606,#9607),.UNSPECIFIED.,.F.,.F.)
B_SPLINE_CURVE_WITH_KNOTS((3,3),(2.01951998481884,2.96895978564587),
 .UNSPECIFIED.)
CURVE()
GEOMETRIC_REPRESENTATION_ITEM()
RATIONAL_B_SPLINE_CURVE((1.48112522432469,1.48112522432469,1.37478521766072))
REPRESENTATION_ITEM('')
);
#119=SHAPE_REPRESENTATION_RELATIONSHIP('SRR','None',#9712,#130);
#120=SHAPE_REPRESENTATION_RELATIONSHIP('SRR','None',#9713,#131);
#121=SHAPE_REPRESENTATION_RELATIONSHIP('SRR','None',#9714,#132);
#122=SHAPE_REPRESENTATION_RELATIONSHIP('SRR','None',#9715,#133);
#123=SHAPE_REPRESENTATION_RELATIONSHIP('SRR','None',#9716,#134);
#124=SHAPE_REPRESENTATION_RELATIONSHIP('SRR','None',#9717,#135);
#125=SHAPE_REPRESENTATION_RELATIONSHIP('SRR','None',#9718,#136);
#126=SHAPE_REPRESENTATION_RELATIONSHIP('SRR','None',#9719,#137);
#127=SHAPE_REPRESENTATION_RELATIONSHIP('SRR','None',#9720,#138);
#128=SHAPE_REPRESENTATION_RELATIONSHIP('SRR','None',#9721,#139);
#129=SHAPE_REPRESENTATION_RELATIONSHIP('SRR','None',#9722,#140);
#130=ADVANCED_BREP_SHAPE_REPRESENTATION('',(#152),#9657);
#131=ADVANCED_BREP_SHAPE_REPRESENTATION('',(#153),#9658);
#132=ADVANCED_BREP_SHAPE_REPRESENTATION('',(#154),#9659);
#133=ADVANCED_BREP_SHAPE_REPRESENTATION('',(#155),#9660);
#134=ADVANCED_BREP_SHAPE_REPRESENTATION('',(#156),#9661);
#135=ADVANCED_BREP_SHAPE_REPRESENTATION('',(#157),#9662);
#136=ADVANCED_BREP_SHAPE_REPRESENTATION('',(#158),#9663);
#137=ADVANCED_BREP_SHAPE_REPRESENTATION('',(#159),#9664);
#138=ADVANCED_BREP_SHAPE_REPRESENTATION('',(#160),#9665);
#139=ADVANCED_BREP_SHAPE_REPRESENTATION('',(#161),#9666);
#140=ADVANCED_BREP_SHAPE_REPRESENTATION('',(#162),#9667);
#141=STYLED_ITEM('',(#9775),#152);
#142=STYLED_ITEM('',(#9775),#153);
#143=STYLED_ITEM('',(#9775),#154);
#144=STYLED_ITEM('',(#9775),#155);
#145=STYLED_ITEM('',(#9775),#156);
#146=STYLED_ITEM('',(#9775),#157);
#147=STYLED_ITEM('',(#9775),#158);
#148=STYLED_ITEM('',(#9775),#159);
#149=STYLED_ITEM('',(#9775),#160);
#150=STYLED_ITEM('',(#9775),#161);
#151=STYLED_ITEM('',(#9775),#162);
#152=MANIFOLD_SOLID_BREP('Body1',#3881);
#153=MANIFOLD_SOLID_BREP('Body1',#3882);
#154=MANIFOLD_SOLID_BREP('Body1',#3883);
#155=MANIFOLD_SOLID_BREP('Body1',#3884);
#156=MANIFOLD_SOLID_BREP('Body1',#3885);
#157=MANIFOLD_SOLID_BREP('Body1',#3886);
#158=MANIFOLD_SOLID_BREP('Body1',#3887);
#159=MANIFOLD_SOLID_BREP('Body1',#3888);
#160=MANIFOLD_SOLID_BREP('Body1',#3889);
#161=MANIFOLD_SOLID_BREP('Body1',#3890);
#162=MANIFOLD_SOLID_BREP('Body1',#3891);
#163=CONICAL_SURFACE('',#4037,30.,0.785398163397447);
#164=CONICAL_SURFACE('',#4125,1000.,1.02974425867666);
#165=CONICAL_SURFACE('',#4162,26.,0.785398163397448);
#166=CONICAL_SURFACE('',#4190,22.,0.785398163397446);
#167=CONICAL_SURFACE('',#4191,22.,0.785398163397446);
#168=CONICAL_SURFACE('',#4192,22.,0.785398163397446);
#169=CONICAL_SURFACE('',#4193,22.,0.785398163397446);
#170=CONICAL_SURFACE('',#4232,2.,0.0178552451395525);
#171=CONICAL_SURFACE('',#4233,2.,0.0178552451395525);
#172=CONICAL_SURFACE('',#4235,1.5,0.0178552451395525);
#173=CONICAL_SURFACE('',#4247,18.,1.1071487177941);
#174=CONICAL_SURFACE('',#4254,19.9999999999999,0.298498931586182);
#175=CONICAL_SURFACE('',#4291,10.,1.10714871779409);
#176=CONICAL_SURFACE('',#4320,34.6410161513776,0.255722691902349);
#177=CONICAL_SURFACE('',#4418,10.3923048454133,0.78539816339745);
#178=CONICAL_SURFACE('',#4419,10.3923048454133,0.78539816339745);
#179=CONICAL_SURFACE('',#4420,10.3923048454133,0.78539816339745);
#180=CONICAL_SURFACE('',#4421,10.3923048454133,0.78539816339745);
#181=CONICAL_SURFACE('',#4422,10.3923048454133,0.78539816339745);
#182=CONICAL_SURFACE('',#4423,10.3923048454133,0.78539816339745);
#183=CONICAL_SURFACE('',#4424,10.3923048454133,0.78539816339745);
#184=CONICAL_SURFACE('',#4425,10.3923048454133,0.78539816339745);
#185=CONICAL_SURFACE('',#4426,10.3923048454133,0.78539816339745);
#186=CONICAL_SURFACE('',#4427,10.3923048454133,0.78539816339745);
#187=CONICAL_SURFACE('',#4428,10.3923048454133,0.78539816339745);
#188=CONICAL_SURFACE('',#4429,10.3923048454133,0.78539816339745);
#189=CONICAL_SURFACE('',#4442,10.3923048454133,0.78539816339745);
#190=CONICAL_SURFACE('',#4444,10.3923048454133,0.78539816339745);
#191=CONICAL_SURFACE('',#4446,10.3923048454133,0.78539816339745);
#192=CONICAL_SURFACE('',#4448,10.3923048454133,0.78539816339745);
#193=CONICAL_SURFACE('',#4450,10.3923048454133,0.78539816339745);
#194=CONICAL_SURFACE('',#4452,10.3923048454133,0.78539816339745);
#195=FACE_BOUND('',#1037,.T.);
#196=FACE_BOUND('',#1038,.T.);
#197=FACE_BOUND('',#1039,.T.);
#198=FACE_BOUND('',#1041,.T.);
#199=FACE_BOUND('',#1045,.T.);
#200=FACE_BOUND('',#1048,.T.);
#201=FACE_BOUND('',#1049,.T.);
#202=FACE_BOUND('',#1050,.T.);
#203=FACE_BOUND('',#1051,.T.);
#204=FACE_BOUND('',#1052,.T.);
#205=FACE_BOUND('',#1055,.T.);
#206=FACE_BOUND('',#1056,.T.);
#207=FACE_BOUND('',#1057,.T.);
#208=FACE_BOUND('',#1058,.T.);
#209=FACE_BOUND('',#1059,.T.);
#210=FACE_BOUND('',#1063,.T.);
#211=FACE_BOUND('',#1068,.T.);
#212=FACE_BOUND('',#1069,.T.);
#213=FACE_BOUND('',#1070,.T.);
#214=FACE_BOUND('',#1071,.T.);
#215=FACE_BOUND('',#1072,.T.);
#216=FACE_BOUND('',#1075,.T.);
#217=FACE_BOUND('',#1077,.T.);
#218=FACE_BOUND('',#1079,.T.);
#219=FACE_BOUND('',#1083,.T.);
#220=FACE_BOUND('',#1084,.T.);
#221=FACE_BOUND('',#1085,.T.);
#222=FACE_BOUND('',#1086,.T.);
#223=FACE_BOUND('',#1087,.T.);
#224=FACE_BOUND('',#1089,.T.);
#225=FACE_BOUND('',#1090,.T.);
#226=FACE_BOUND('',#1091,.T.);
#227=FACE_BOUND('',#1092,.T.);
#228=FACE_BOUND('',#1093,.T.);
#229=FACE_BOUND('',#1124,.T.);
#230=FACE_BOUND('',#1127,.T.);
#231=FACE_BOUND('',#1128,.T.);
#232=FACE_BOUND('',#1133,.T.);
#233=FACE_BOUND('',#1154,.T.);
#234=FACE_BOUND('',#1157,.T.);
#235=FACE_BOUND('',#1159,.T.);
#236=FACE_BOUND('',#1160,.T.);
#237=FACE_BOUND('',#1171,.T.);
#238=FACE_BOUND('',#1173,.T.);
#239=FACE_BOUND('',#1175,.T.);
#240=FACE_BOUND('',#1177,.T.);
#241=FACE_BOUND('',#1184,.T.);
#242=FACE_BOUND('',#1189,.T.);
#243=FACE_BOUND('',#1192,.T.);
#244=FACE_BOUND('',#1195,.T.);
#245=FACE_BOUND('',#1196,.T.);
#246=FACE_BOUND('',#1197,.T.);
#247=FACE_BOUND('',#1198,.T.);
#248=FACE_BOUND('',#1199,.T.);
#249=FACE_BOUND('',#1202,.T.);
#250=FACE_BOUND('',#1203,.T.);
#251=FACE_BOUND('',#1204,.T.);
#252=FACE_BOUND('',#1205,.T.);
#253=FACE_BOUND('',#1206,.T.);
#254=FACE_BOUND('',#1214,.T.);
#255=FACE_BOUND('',#1217,.T.);
#256=FACE_BOUND('',#1227,.T.);
#257=FACE_BOUND('',#1230,.T.);
#258=FACE_BOUND('',#1238,.T.);
#259=FACE_BOUND('',#1242,.T.);
#260=FACE_BOUND('',#1262,.T.);
#261=FACE_BOUND('',#1263,.T.);
#262=FACE_BOUND('',#1264,.T.);
#263=FACE_BOUND('',#1266,.T.);
#264=FACE_BOUND('',#1268,.T.);
#265=FACE_BOUND('',#1296,.T.);
#266=FACE_BOUND('',#1298,.T.);
#267=FACE_BOUND('',#1321,.T.);
#268=PLANE('',#4028);
#269=PLANE('',#4034);
#270=PLANE('',#4042);
#271=PLANE('',#4046);
#272=PLANE('',#4055);
#273=PLANE('',#4068);
#274=PLANE('',#4078);
#275=PLANE('',#4088);
#276=PLANE('',#4092);
#277=PLANE('',#4099);
#278=PLANE('',#4104);
#279=PLANE('',#4111);
#280=PLANE('',#4112);
#281=PLANE('',#4136);
#282=PLANE('',#4138);
#283=PLANE('',#4140);
#284=PLANE('',#4142);
#285=PLANE('',#4144);
#286=PLANE('',#4145);
#287=PLANE('',#4146);
#288=PLANE('',#4147);
#289=PLANE('',#4148);
#290=PLANE('',#4157);
#291=PLANE('',#4168);
#292=PLANE('',#4169);
#293=PLANE('',#4171);
#294=PLANE('',#4177);
#295=PLANE('',#4182);
#296=PLANE('',#4183);
#297=PLANE('',#4186);
#298=PLANE('',#4187);
#299=PLANE('',#4195);
#300=PLANE('',#4197);
#301=PLANE('',#4199);
#302=PLANE('',#4201);
#303=PLANE('',#4203);
#304=PLANE('',#4207);
#305=PLANE('',#4214);
#306=PLANE('',#4215);
#307=PLANE('',#4216);
#308=PLANE('',#4217);
#309=PLANE('',#4218);
#310=PLANE('',#4222);
#311=PLANE('',#4224);
#312=PLANE('',#4227);
#313=PLANE('',#4238);
#314=PLANE('',#4239);
#315=PLANE('',#4241);
#316=PLANE('',#4252);
#317=PLANE('',#4256);
#318=PLANE('',#4260);
#319=PLANE('',#4268);
#320=PLANE('',#4283);
#321=PLANE('',#4287);
#322=PLANE('',#4293);
#323=PLANE('',#4294);
#324=PLANE('',#4295);
#325=PLANE('',#4296);
#326=PLANE('',#4297);
#327=PLANE('',#4298);
#328=PLANE('',#4299);
#329=PLANE('',#4303);
#330=PLANE('',#4317);
#331=PLANE('',#4323);
#332=PLANE('',#4327);
#333=PLANE('',#4328);
#334=PLANE('',#4329);
#335=PLANE('',#4332);
#336=PLANE('',#4336);
#337=PLANE('',#4339);
#338=PLANE('',#4343);
#339=PLANE('',#4346);
#340=PLANE('',#4349);
#341=PLANE('',#4350);
#342=PLANE('',#4351);
#343=PLANE('',#4352);
#344=PLANE('',#4353);
#345=PLANE('',#4354);
#346=PLANE('',#4363);
#347=PLANE('',#4365);
#348=PLANE('',#4380);
#349=PLANE('',#4381);
#350=PLANE('',#4382);
#351=PLANE('',#4383);
#352=PLANE('',#4384);
#353=PLANE('',#4385);
#354=PLANE('',#4395);
#355=PLANE('',#4396);
#356=PLANE('',#4397);
#357=PLANE('',#4398);
#358=PLANE('',#4399);
#359=PLANE('',#4400);
#360=PLANE('',#4401);
#361=PLANE('',#4409);
#362=PLANE('',#4431);
#363=PLANE('',#4432);
#364=PLANE('',#4433);
#365=PLANE('',#4434);
#366=PLANE('',#4435);
#367=PLANE('',#4436);
#368=PLANE('',#4440);
#369=PLANE('',#4441);
#370=PLANE('',#4454);
#371=LINE('',#5637,#562);
#372=LINE('',#5688,#563);
#373=LINE('',#5690,#564);
#374=LINE('',#5995,#565);
#375=LINE('',#5997,#566);
#376=LINE('',#6015,#567);
#377=LINE('',#6018,#568);
#378=LINE('',#6025,#569);
#379=LINE('',#6040,#570);
#380=LINE('',#6059,#571);
#381=LINE('',#6078,#572);
#382=LINE('',#6080,#573);
#383=LINE('',#6082,#574);
#384=LINE('',#6084,#575);
#385=LINE('',#6102,#576);
#386=LINE('',#6109,#577);
#387=LINE('',#6190,#578);
#388=LINE('',#6213,#579);
#389=LINE('',#6214,#580);
#390=LINE('',#6216,#581);
#391=LINE('',#6218,#582);
#392=LINE('',#6220,#583);
#393=LINE('',#6222,#584);
#394=LINE('',#6224,#585);
#395=LINE('',#6226,#586);
#396=LINE('',#6228,#587);
#397=LINE('',#6230,#588);
#398=LINE('',#6232,#589);
#399=LINE('',#6234,#590);
#400=LINE('',#6236,#591);
#401=LINE('',#6239,#592);
#402=LINE('',#6245,#593);
#403=LINE('',#6247,#594);
#404=LINE('',#6249,#595);
#405=LINE('',#6251,#596);
#406=LINE('',#6264,#597);
#407=LINE('',#6265,#598);
#408=LINE('',#6269,#599);
#409=LINE('',#6271,#600);
#410=LINE('',#6276,#601);
#411=LINE('',#6278,#602);
#412=LINE('',#6285,#603);
#413=LINE('',#6286,#604);
#414=LINE('',#6289,#605);
#415=LINE('',#6295,#606);
#416=LINE('',#6296,#607);
#417=LINE('',#6300,#608);
#418=LINE('',#6305,#609);
#419=LINE('',#6306,#610);
#420=LINE('',#6310,#611);
#421=LINE('',#6315,#612);
#422=LINE('',#6316,#613);
#423=LINE('',#6319,#614);
#424=LINE('',#6325,#615);
#425=LINE('',#6326,#616);
#426=LINE('',#6335,#617);
#427=LINE('',#6338,#618);
#428=LINE('',#6342,#619);
#429=LINE('',#6346,#620);
#430=LINE('',#6350,#621);
#431=LINE('',#6355,#622);
#432=LINE('',#6356,#623);
#433=LINE('',#6362,#624);
#434=LINE('',#6365,#625);
#435=LINE('',#6372,#626);
#436=LINE('',#6374,#627);
#437=LINE('',#6379,#628);
#438=LINE('',#6386,#629);
#439=LINE('',#6389,#630);
#440=LINE('',#6392,#631);
#441=LINE('',#6395,#632);
#442=LINE('',#6402,#633);
#443=LINE('',#6405,#634);
#444=LINE('',#6416,#635);
#445=LINE('',#6419,#636);
#446=LINE('',#6435,#637);
#447=LINE('',#6436,#638);
#448=LINE('',#6441,#639);
#449=LINE('',#6442,#640);
#450=LINE('',#6447,#641);
#451=LINE('',#6448,#642);
#452=LINE('',#6457,#643);
#453=LINE('',#6459,#644);
#454=LINE('',#6461,#645);
#455=LINE('',#6462,#646);
#456=LINE('',#6466,#647);
#457=LINE('',#6473,#648);
#458=LINE('',#6551,#649);
#459=LINE('',#6555,#650);
#460=LINE('',#6557,#651);
#461=LINE('',#6558,#652);
#462=LINE('',#6560,#653);
#463=LINE('',#6562,#654);
#464=LINE('',#6564,#655);
#465=LINE('',#6569,#656);
#466=LINE('',#6585,#657);
#467=LINE('',#6613,#658);
#468=LINE('',#6674,#659);
#469=LINE('',#6702,#660);
#470=LINE('',#6762,#661);
#471=LINE('',#6764,#662);
#472=LINE('',#6770,#663);
#473=LINE('',#6782,#664);
#474=LINE('',#6791,#665);
#475=LINE('',#6794,#666);
#476=LINE('',#6802,#667);
#477=LINE('',#6808,#668);
#478=LINE('',#6823,#669);
#479=LINE('',#6837,#670);
#480=LINE('',#6839,#671);
#481=LINE('',#6841,#672);
#482=LINE('',#6843,#673);
#483=LINE('',#6845,#674);
#484=LINE('',#6851,#675);
#485=LINE('',#6859,#676);
#486=LINE('',#6866,#677);
#487=LINE('',#6868,#678);
#488=LINE('',#6873,#679);
#489=LINE('',#6921,#680);
#490=LINE('',#6922,#681);
#491=LINE('',#6926,#682);
#492=LINE('',#6964,#683);
#493=LINE('',#7005,#684);
#494=LINE('',#7006,#685);
#495=LINE('',#7010,#686);
#496=LINE('',#7048,#687);
#497=LINE('',#7052,#688);
#498=LINE('',#7090,#689);
#499=LINE('',#7129,#690);
#500=LINE('',#7136,#691);
#501=LINE('',#7158,#692);
#502=LINE('',#7162,#693);
#503=LINE('',#7167,#694);
#504=LINE('',#7172,#695);
#505=LINE('',#7263,#696);
#506=LINE('',#7276,#697);
#507=LINE('',#7290,#698);
#508=LINE('',#7384,#699);
#509=LINE('',#7397,#700);
#510=LINE('',#7440,#701);
#511=LINE('',#7444,#702);
#512=LINE('',#7477,#703);
#513=LINE('',#7481,#704);
#514=LINE('',#7512,#705);
#515=LINE('',#7516,#706);
#516=LINE('',#7578,#707);
#517=LINE('',#7582,#708);
#518=LINE('',#7701,#709);
#519=LINE('',#7714,#710);
#520=LINE('',#7728,#711);
#521=LINE('',#7823,#712);
#522=LINE('',#7932,#713);
#523=LINE('',#8044,#714);
#524=LINE('',#8149,#715);
#525=LINE('',#8162,#716);
#526=LINE('',#8176,#717);
#527=LINE('',#8274,#718);
#528=LINE('',#8925,#719);
#529=LINE('',#8930,#720);
#530=LINE('',#8943,#721);
#531=LINE('',#8945,#722);
#532=LINE('',#8947,#723);
#533=LINE('',#8948,#724);
#534=LINE('',#8952,#725);
#535=LINE('',#8954,#726);
#536=LINE('',#8956,#727);
#537=LINE('',#8957,#728);
#538=LINE('',#8959,#729);
#539=LINE('',#8960,#730);
#540=LINE('',#8962,#731);
#541=LINE('',#8964,#732);
#542=LINE('',#9402,#733);
#543=LINE('',#9412,#734);
#544=LINE('',#9423,#735);
#545=LINE('',#9441,#736);
#546=LINE('',#9459,#737);
#547=LINE('',#9477,#738);
#548=LINE('',#9522,#739);
#549=LINE('',#9543,#740);
#550=LINE('',#9545,#741);
#551=LINE('',#9547,#742);
#552=LINE('',#9557,#743);
#553=LINE('',#9559,#744);
#554=LINE('',#9569,#745);
#555=LINE('',#9571,#746);
#556=LINE('',#9581,#747);
#557=LINE('',#9583,#748);
#558=LINE('',#9593,#749);
#559=LINE('',#9595,#750);
#560=LINE('',#9604,#751);
#561=LINE('',#9612,#752);
#562=VECTOR('',#4483,18.3303029094034);
#563=VECTOR('',#4484,38.);
#564=VECTOR('',#4487,18.3303193041542);
#565=VECTOR('',#4504,15.6464703888607);
#566=VECTOR('',#4505,15.6464703888607);
#567=VECTOR('',#4526,30.);
#568=VECTOR('',#4529,26.);
#569=VECTOR('',#4538,23.9999999999998);
#570=VECTOR('',#4555,83.9999999999998);
#571=VECTOR('',#4576,39.9999999999999);
#572=VECTOR('',#4603,56.0000000000001);
#573=VECTOR('',#4606,7.94448724536034);
#574=VECTOR('',#4607,90.0000000000003);
#575=VECTOR('',#4610,7.94448724536034);
#576=VECTOR('',#4629,39.999999999998);
#577=VECTOR('',#4638,44.0000000000001);
#578=VECTOR('',#4653,84.);
#579=VECTOR('',#4680,40.0090835271346);
#580=VECTOR('',#4681,40.011431530049);
#581=VECTOR('',#4684,42.);
#582=VECTOR('',#4687,42.);
#583=VECTOR('',#4690,24.);
#584=VECTOR('',#4693,8.);
#585=VECTOR('',#4696,8.);
#586=VECTOR('',#4699,8.);
#587=VECTOR('',#4702,8.);
#588=VECTOR('',#4705,8.);
#589=VECTOR('',#4708,8.);
#590=VECTOR('',#4711,8.);
#591=VECTOR('',#4714,8.);
#592=VECTOR('',#4717,6.00000000000001);
#593=VECTOR('',#4724,1000.);
#594=VECTOR('',#4727,6.00000000000001);
#595=VECTOR('',#4730,6.00000000000001);
#596=VECTOR('',#4733,6.00000000000001);
#597=VECTOR('',#4752,23.9229627936314);
#598=VECTOR('',#4753,23.9229627936314);
#599=VECTOR('',#4756,23.9229627936314);
#600=VECTOR('',#4757,23.9229627936314);
#601=VECTOR('',#4762,23.9229627936314);
#602=VECTOR('',#4763,23.9229627936314);
#603=VECTOR('',#4770,23.9229627936314);
#604=VECTOR('',#4771,23.9229627936314);
#605=VECTOR('',#4774,20.);
#606=VECTOR('',#4775,19.9089023002066);
#607=VECTOR('',#4776,24.);
#608=VECTOR('',#4779,19.9089023002066);
#609=VECTOR('',#4780,20.);
#610=VECTOR('',#4781,24.);
#611=VECTOR('',#4784,19.9089023002066);
#612=VECTOR('',#4785,20.);
#613=VECTOR('',#4786,24.);
#614=VECTOR('',#4789,20.);
#615=VECTOR('',#4790,19.9089023002066);
#616=VECTOR('',#4791,24.);
#617=VECTOR('',#4800,16.);
#618=VECTOR('',#4803,24.);
#619=VECTOR('',#4806,16.);
#620=VECTOR('',#4809,16.);
#621=VECTOR('',#4812,16.);
#622=VECTOR('',#4819,35.7770876399966);
#623=VECTOR('',#4820,35.7770876399966);
#624=VECTOR('',#4827,30.);
#625=VECTOR('',#4830,26.);
#626=VECTOR('',#4843,35.7770876399966);
#627=VECTOR('',#4846,35.7770876399966);
#628=VECTOR('',#4853,11.);
#629=VECTOR('',#4864,19.9089023002066);
#630=VECTOR('',#4867,19.9089023002066);
#631=VECTOR('',#4870,19.9089023002066);
#632=VECTOR('',#4873,19.9089023002066);
#633=VECTOR('',#4878,20.);
#634=VECTOR('',#4881,20.);
#635=VECTOR('',#4888,20.);
#636=VECTOR('',#4891,20.);
#637=VECTOR('',#4910,6.);
#638=VECTOR('',#4911,6.);
#639=VECTOR('',#4916,6.);
#640=VECTOR('',#4917,6.);
#641=VECTOR('',#4922,6.);
#642=VECTOR('',#4923,6.);
#643=VECTOR('',#4932,12.);
#644=VECTOR('',#4933,12.);
#645=VECTOR('',#4934,12.);
#646=VECTOR('',#4935,12.);
#647=VECTOR('',#4940,9.99999999999998);
#648=VECTOR('',#4949,8.);
#649=VECTOR('',#4952,2.);
#650=VECTOR('',#4959,16.);
#651=VECTOR('',#4960,6.);
#652=VECTOR('',#4961,16.);
#653=VECTOR('',#4964,16.);
#654=VECTOR('',#4967,16.);
#655=VECTOR('',#4970,6.);
#656=VECTOR('',#4977,6.);
#657=VECTOR('',#4998,14.);
#658=VECTOR('',#4999,14.);
#659=VECTOR('',#5002,8.);
#660=VECTOR('',#5003,8.);
#661=VECTOR('',#5006,2.);
#662=VECTOR('',#5009,2.);
#663=VECTOR('',#5016,1.5);
#664=VECTOR('',#5033,18.0000000000001);
#665=VECTOR('',#5044,18.);
#666=VECTOR('',#5047,9.99999999999995);
#667=VECTOR('',#5058,19.9999999999999);
#668=VECTOR('',#5065,40.);
#669=VECTOR('',#5082,89.999999999998);
#670=VECTOR('',#5099,25.999999999998);
#671=VECTOR('',#5102,6.);
#672=VECTOR('',#5105,6.);
#673=VECTOR('',#5108,6.);
#674=VECTOR('',#5111,6.);
#675=VECTOR('',#5118,10.);
#676=VECTOR('',#5129,22.0000000000001);
#677=VECTOR('',#5138,18.);
#678=VECTOR('',#5141,10.);
#679=VECTOR('',#5146,34.6410161513776);
#680=VECTOR('',#5147,34.6410161513776);
#681=VECTOR('',#5148,39.9999999999996);
#682=VECTOR('',#5151,34.6410161513776);
#683=VECTOR('',#5152,40.0000000000001);
#684=VECTOR('',#5155,40.0000000000001);
#685=VECTOR('',#5156,34.6410161513776);
#686=VECTOR('',#5159,34.6410161513776);
#687=VECTOR('',#5160,40.0000000000001);
#688=VECTOR('',#5163,34.6410161513776);
#689=VECTOR('',#5164,40.0000000000001);
#690=VECTOR('',#5167,40.0000000000001);
#691=VECTOR('',#5176,26.);
#692=VECTOR('',#5213,34.6410161513776);
#693=VECTOR('',#5218,12.);
#694=VECTOR('',#5225,10.);
#695=VECTOR('',#5230,51.1691161062453);
#696=VECTOR('',#5231,51.1691161062453);
#697=VECTOR('',#5232,16.);
#698=VECTOR('',#5235,51.1691161062453);
#699=VECTOR('',#5236,51.1691161062453);
#700=VECTOR('',#5237,16.);
#701=VECTOR('',#5246,51.1691161062453);
#702=VECTOR('',#5249,51.1691161062452);
#703=VECTOR('',#5256,51.1691161062453);
#704=VECTOR('',#5259,51.1691161062453);
#705=VECTOR('',#5264,51.1691161062453);
#706=VECTOR('',#5267,51.1691161062453);
#707=VECTOR('',#5280,51.1691161062453);
#708=VECTOR('',#5283,51.1691161062453);
#709=VECTOR('',#5288,51.1691161062453);
#710=VECTOR('',#5289,16.);
#711=VECTOR('',#5292,51.1691161062453);
#712=VECTOR('',#5293,16.);
#713=VECTOR('',#5296,16.);
#714=VECTOR('',#5299,16.);
#715=VECTOR('',#5302,51.1691161062453);
#716=VECTOR('',#5303,16.);
#717=VECTOR('',#5306,51.1691161062453);
#718=VECTOR('',#5307,16.);
#719=VECTOR('',#5336,16.);
#720=VECTOR('',#5341,16.);
#721=VECTOR('',#5362,12.);
#722=VECTOR('',#5363,12.);
#723=VECTOR('',#5364,12.);
#724=VECTOR('',#5365,12.);
#725=VECTOR('',#5368,12.);
#726=VECTOR('',#5369,12.);
#727=VECTOR('',#5370,12.);
#728=VECTOR('',#5371,12.);
#729=VECTOR('',#5374,20.);
#730=VECTOR('',#5375,20.);
#731=VECTOR('',#5378,20.);
#732=VECTOR('',#5381,20.);
#733=VECTOR('',#5404,8.78460969082654);
#734=VECTOR('',#5405,8.78460969082657);
#735=VECTOR('',#5408,8.78460969082654);
#736=VECTOR('',#5411,8.78460969082653);
#737=VECTOR('',#5414,8.78460969082654);
#738=VECTOR('',#5417,8.78460969082654);
#739=VECTOR('',#5454,6.);
#740=VECTOR('',#5483,7.39230484541327);
#741=VECTOR('',#5484,12.);
#742=VECTOR('',#5485,7.39230484541327);
#743=VECTOR('',#5488,12.);
#744=VECTOR('',#5489,7.39230484541327);
#745=VECTOR('',#5492,12.);
#746=VECTOR('',#5493,7.39230484541327);
#747=VECTOR('',#5496,12.);
#748=VECTOR('',#5497,7.39230484541327);
#749=VECTOR('',#5500,12.);
#750=VECTOR('',#5501,7.39230484541327);
#751=VECTOR('',#5504,12.);
#752=VECTOR('',#5509,6.);
#753=CYLINDRICAL_SURFACE('',#4020,38.);
#754=CYLINDRICAL_SURFACE('',#4040,26.);
#755=CYLINDRICAL_SURFACE('',#4044,23.9999999999998);
#756=CYLINDRICAL_SURFACE('',#4052,83.9999999999998);
#757=CYLINDRICAL_SURFACE('',#4062,39.9999999999999);
#758=CYLINDRICAL_SURFACE('',#4075,56.0000000000001);
#759=CYLINDRICAL_SURFACE('',#4076,90.0000000000003);
#760=CYLINDRICAL_SURFACE('',#4084,39.999999999998);
#761=CYLINDRICAL_SURFACE('',#4090,44.0000000000001);
#762=CYLINDRICAL_SURFACE('',#4096,84.);
#763=CYLINDRICAL_SURFACE('',#4110,56.);
#764=CYLINDRICAL_SURFACE('',#4113,24.);
#765=CYLINDRICAL_SURFACE('',#4114,8.);
#766=CYLINDRICAL_SURFACE('',#4115,8.);
#767=CYLINDRICAL_SURFACE('',#4116,8.);
#768=CYLINDRICAL_SURFACE('',#4117,8.);
#769=CYLINDRICAL_SURFACE('',#4118,8.);
#770=CYLINDRICAL_SURFACE('',#4119,8.);
#771=CYLINDRICAL_SURFACE('',#4120,8.);
#772=CYLINDRICAL_SURFACE('',#4121,8.);
#773=CYLINDRICAL_SURFACE('',#4122,6.00000000000001);
#774=CYLINDRICAL_SURFACE('',#4126,6.00000000000001);
#775=CYLINDRICAL_SURFACE('',#4127,6.00000000000001);
#776=CYLINDRICAL_SURFACE('',#4128,6.00000000000001);
#777=CYLINDRICAL_SURFACE('',#4129,30.);
#778=CYLINDRICAL_SURFACE('',#4130,30.);
#779=CYLINDRICAL_SURFACE('',#4151,24.);
#780=CYLINDRICAL_SURFACE('',#4159,30.);
#781=CYLINDRICAL_SURFACE('',#4172,11.);
#782=CYLINDRICAL_SURFACE('',#4173,26.);
#783=CYLINDRICAL_SURFACE('',#4175,26.);
#784=CYLINDRICAL_SURFACE('',#4184,26.);
#785=CYLINDRICAL_SURFACE('',#4188,26.);
#786=CYLINDRICAL_SURFACE('',#4205,9.99999999999998);
#787=CYLINDRICAL_SURFACE('',#4209,8.);
#788=CYLINDRICAL_SURFACE('',#4211,2.);
#789=CYLINDRICAL_SURFACE('',#4220,6.);
#790=CYLINDRICAL_SURFACE('',#4230,14.);
#791=CYLINDRICAL_SURFACE('',#4231,8.);
#792=CYLINDRICAL_SURFACE('',#4244,18.0000000000001);
#793=CYLINDRICAL_SURFACE('',#4250,9.99999999999995);
#794=CYLINDRICAL_SURFACE('',#4258,40.);
#795=CYLINDRICAL_SURFACE('',#4266,89.999999999998);
#796=CYLINDRICAL_SURFACE('',#4274,25.999999999998);
#797=CYLINDRICAL_SURFACE('',#4275,6.);
#798=CYLINDRICAL_SURFACE('',#4276,6.);
#799=CYLINDRICAL_SURFACE('',#4277,6.);
#800=CYLINDRICAL_SURFACE('',#4278,6.);
#801=CYLINDRICAL_SURFACE('',#4280,10.);
#802=CYLINDRICAL_SURFACE('',#4285,22.0000000000001);
#803=CYLINDRICAL_SURFACE('',#4289,18.);
#804=CYLINDRICAL_SURFACE('',#4301,26.);
#805=CYLINDRICAL_SURFACE('',#4321,12.);
#806=CYLINDRICAL_SURFACE('',#4325,10.);
#807=CYLINDRICAL_SURFACE('',#4367,16.);
#808=CYLINDRICAL_SURFACE('',#4417,6.);
#809=CYLINDRICAL_SURFACE('',#4437,6.);
#810=FACE_OUTER_BOUND('',#1033,.T.);
#811=FACE_OUTER_BOUND('',#1034,.T.);
#812=FACE_OUTER_BOUND('',#1035,.T.);
#813=FACE_OUTER_BOUND('',#1036,.T.);
#814=FACE_OUTER_BOUND('',#1040,.T.);
#815=FACE_OUTER_BOUND('',#1042,.T.);
#816=FACE_OUTER_BOUND('',#1043,.T.);
#817=FACE_OUTER_BOUND('',#1044,.T.);
#818=FACE_OUTER_BOUND('',#1046,.T.);
#819=FACE_OUTER_BOUND('',#1047,.T.);
#820=FACE_OUTER_BOUND('',#1053,.T.);
#821=FACE_OUTER_BOUND('',#1054,.T.);
#822=FACE_OUTER_BOUND('',#1060,.T.);
#823=FACE_OUTER_BOUND('',#1061,.T.);
#824=FACE_OUTER_BOUND('',#1062,.T.);
#825=FACE_OUTER_BOUND('',#1064,.T.);
#826=FACE_OUTER_BOUND('',#1065,.T.);
#827=FACE_OUTER_BOUND('',#1066,.T.);
#828=FACE_OUTER_BOUND('',#1067,.T.);
#829=FACE_OUTER_BOUND('',#1073,.T.);
#830=FACE_OUTER_BOUND('',#1074,.T.);
#831=FACE_OUTER_BOUND('',#1076,.T.);
#832=FACE_OUTER_BOUND('',#1078,.T.);
#833=FACE_OUTER_BOUND('',#1080,.T.);
#834=FACE_OUTER_BOUND('',#1081,.T.);
#835=FACE_OUTER_BOUND('',#1082,.T.);
#836=FACE_OUTER_BOUND('',#1088,.T.);
#837=FACE_OUTER_BOUND('',#1094,.T.);
#838=FACE_OUTER_BOUND('',#1095,.T.);
#839=FACE_OUTER_BOUND('',#1096,.T.);
#840=FACE_OUTER_BOUND('',#1097,.T.);
#841=FACE_OUTER_BOUND('',#1098,.T.);
#842=FACE_OUTER_BOUND('',#1099,.T.);
#843=FACE_OUTER_BOUND('',#1100,.T.);
#844=FACE_OUTER_BOUND('',#1101,.T.);
#845=FACE_OUTER_BOUND('',#1102,.T.);
#846=FACE_OUTER_BOUND('',#1103,.T.);
#847=FACE_OUTER_BOUND('',#1104,.T.);
#848=FACE_OUTER_BOUND('',#1105,.T.);
#849=FACE_OUTER_BOUND('',#1106,.T.);
#850=FACE_OUTER_BOUND('',#1107,.T.);
#851=FACE_OUTER_BOUND('',#1108,.T.);
#852=FACE_OUTER_BOUND('',#1109,.T.);
#853=FACE_OUTER_BOUND('',#1110,.T.);
#854=FACE_OUTER_BOUND('',#1111,.T.);
#855=FACE_OUTER_BOUND('',#1112,.T.);
#856=FACE_OUTER_BOUND('',#1113,.T.);
#857=FACE_OUTER_BOUND('',#1114,.T.);
#858=FACE_OUTER_BOUND('',#1115,.T.);
#859=FACE_OUTER_BOUND('',#1116,.T.);
#860=FACE_OUTER_BOUND('',#1117,.T.);
#861=FACE_OUTER_BOUND('',#1118,.T.);
#862=FACE_OUTER_BOUND('',#1119,.T.);
#863=FACE_OUTER_BOUND('',#1120,.T.);
#864=FACE_OUTER_BOUND('',#1121,.T.);
#865=FACE_OUTER_BOUND('',#1122,.T.);
#866=FACE_OUTER_BOUND('',#1123,.T.);
#867=FACE_OUTER_BOUND('',#1125,.T.);
#868=FACE_OUTER_BOUND('',#1126,.T.);
#869=FACE_OUTER_BOUND('',#1129,.T.);
#870=FACE_OUTER_BOUND('',#1130,.T.);
#871=FACE_OUTER_BOUND('',#1131,.T.);
#872=FACE_OUTER_BOUND('',#1132,.T.);
#873=FACE_OUTER_BOUND('',#1134,.T.);
#874=FACE_OUTER_BOUND('',#1135,.T.);
#875=FACE_OUTER_BOUND('',#1136,.T.);
#876=FACE_OUTER_BOUND('',#1137,.T.);
#877=FACE_OUTER_BOUND('',#1138,.T.);
#878=FACE_OUTER_BOUND('',#1139,.T.);
#879=FACE_OUTER_BOUND('',#1140,.T.);
#880=FACE_OUTER_BOUND('',#1141,.T.);
#881=FACE_OUTER_BOUND('',#1142,.T.);
#882=FACE_OUTER_BOUND('',#1143,.T.);
#883=FACE_OUTER_BOUND('',#1144,.T.);
#884=FACE_OUTER_BOUND('',#1145,.T.);
#885=FACE_OUTER_BOUND('',#1146,.T.);
#886=FACE_OUTER_BOUND('',#1147,.T.);
#887=FACE_OUTER_BOUND('',#1148,.T.);
#888=FACE_OUTER_BOUND('',#1149,.T.);
#889=FACE_OUTER_BOUND('',#1150,.T.);
#890=FACE_OUTER_BOUND('',#1151,.T.);
#891=FACE_OUTER_BOUND('',#1152,.T.);
#892=FACE_OUTER_BOUND('',#1153,.T.);
#893=FACE_OUTER_BOUND('',#1155,.T.);
#894=FACE_OUTER_BOUND('',#1156,.T.);
#895=FACE_OUTER_BOUND('',#1158,.T.);
#896=FACE_OUTER_BOUND('',#1161,.T.);
#897=FACE_OUTER_BOUND('',#1162,.T.);
#898=FACE_OUTER_BOUND('',#1163,.T.);
#899=FACE_OUTER_BOUND('',#1164,.T.);
#900=FACE_OUTER_BOUND('',#1165,.T.);
#901=FACE_OUTER_BOUND('',#1166,.T.);
#902=FACE_OUTER_BOUND('',#1167,.T.);
#903=FACE_OUTER_BOUND('',#1168,.T.);
#904=FACE_OUTER_BOUND('',#1169,.T.);
#905=FACE_OUTER_BOUND('',#1170,.T.);
#906=FACE_OUTER_BOUND('',#1172,.T.);
#907=FACE_OUTER_BOUND('',#1174,.T.);
#908=FACE_OUTER_BOUND('',#1176,.T.);
#909=FACE_OUTER_BOUND('',#1178,.T.);
#910=FACE_OUTER_BOUND('',#1179,.T.);
#911=FACE_OUTER_BOUND('',#1180,.T.);
#912=FACE_OUTER_BOUND('',#1181,.T.);
#913=FACE_OUTER_BOUND('',#1182,.T.);
#914=FACE_OUTER_BOUND('',#1183,.T.);
#915=FACE_OUTER_BOUND('',#1185,.T.);
#916=FACE_OUTER_BOUND('',#1186,.T.);
#917=FACE_OUTER_BOUND('',#1187,.T.);
#918=FACE_OUTER_BOUND('',#1188,.T.);
#919=FACE_OUTER_BOUND('',#1190,.T.);
#920=FACE_OUTER_BOUND('',#1191,.T.);
#921=FACE_OUTER_BOUND('',#1193,.T.);
#922=FACE_OUTER_BOUND('',#1194,.T.);
#923=FACE_OUTER_BOUND('',#1200,.T.);
#924=FACE_OUTER_BOUND('',#1201,.T.);
#925=FACE_OUTER_BOUND('',#1207,.T.);
#926=FACE_OUTER_BOUND('',#1208,.T.);
#927=FACE_OUTER_BOUND('',#1209,.T.);
#928=FACE_OUTER_BOUND('',#1210,.T.);
#929=FACE_OUTER_BOUND('',#1211,.T.);
#930=FACE_OUTER_BOUND('',#1212,.T.);
#931=FACE_OUTER_BOUND('',#1213,.T.);
#932=FACE_OUTER_BOUND('',#1215,.T.);
#933=FACE_OUTER_BOUND('',#1216,.T.);
#934=FACE_OUTER_BOUND('',#1218,.T.);
#935=FACE_OUTER_BOUND('',#1219,.T.);
#936=FACE_OUTER_BOUND('',#1220,.T.);
#937=FACE_OUTER_BOUND('',#1221,.T.);
#938=FACE_OUTER_BOUND('',#1222,.T.);
#939=FACE_OUTER_BOUND('',#1223,.T.);
#940=FACE_OUTER_BOUND('',#1224,.T.);
#941=FACE_OUTER_BOUND('',#1225,.T.);
#942=FACE_OUTER_BOUND('',#1226,.T.);
#943=FACE_OUTER_BOUND('',#1228,.T.);
#944=FACE_OUTER_BOUND('',#1229,.T.);
#945=FACE_OUTER_BOUND('',#1231,.T.);
#946=FACE_OUTER_BOUND('',#1232,.T.);
#947=FACE_OUTER_BOUND('',#1233,.T.);
#948=FACE_OUTER_BOUND('',#1234,.T.);
#949=FACE_OUTER_BOUND('',#1235,.T.);
#950=FACE_OUTER_BOUND('',#1236,.T.);
#951=FACE_OUTER_BOUND('',#1237,.T.);
#952=FACE_OUTER_BOUND('',#1239,.T.);
#953=FACE_OUTER_BOUND('',#1240,.T.);
#954=FACE_OUTER_BOUND('',#1241,.T.);
#955=FACE_OUTER_BOUND('',#1243,.T.);
#956=FACE_OUTER_BOUND('',#1244,.T.);
#957=FACE_OUTER_BOUND('',#1245,.T.);
#958=FACE_OUTER_BOUND('',#1246,.T.);
#959=FACE_OUTER_BOUND('',#1247,.T.);
#960=FACE_OUTER_BOUND('',#1248,.T.);
#961=FACE_OUTER_BOUND('',#1249,.T.);
#962=FACE_OUTER_BOUND('',#1250,.T.);
#963=FACE_OUTER_BOUND('',#1251,.T.);
#964=FACE_OUTER_BOUND('',#1252,.T.);
#965=FACE_OUTER_BOUND('',#1253,.T.);
#966=FACE_OUTER_BOUND('',#1254,.T.);
#967=FACE_OUTER_BOUND('',#1255,.T.);
#968=FACE_OUTER_BOUND('',#1256,.T.);
#969=FACE_OUTER_BOUND('',#1257,.T.);
#970=FACE_OUTER_BOUND('',#1258,.T.);
#971=FACE_OUTER_BOUND('',#1259,.T.);
#972=FACE_OUTER_BOUND('',#1260,.T.);
#973=FACE_OUTER_BOUND('',#1261,.T.);
#974=FACE_OUTER_BOUND('',#1265,.T.);
#975=FACE_OUTER_BOUND('',#1267,.T.);
#976=FACE_OUTER_BOUND('',#1269,.T.);
#977=FACE_OUTER_BOUND('',#1270,.T.);
#978=FACE_OUTER_BOUND('',#1271,.T.);
#979=FACE_OUTER_BOUND('',#1272,.T.);
#980=FACE_OUTER_BOUND('',#1273,.T.);
#981=FACE_OUTER_BOUND('',#1274,.T.);
#982=FACE_OUTER_BOUND('',#1275,.T.);
#983=FACE_OUTER_BOUND('',#1276,.T.);
#984=FACE_OUTER_BOUND('',#1277,.T.);
#985=FACE_OUTER_BOUND('',#1278,.T.);
#986=FACE_OUTER_BOUND('',#1279,.T.);
#987=FACE_OUTER_BOUND('',#1280,.T.);
#988=FACE_OUTER_BOUND('',#1281,.T.);
#989=FACE_OUTER_BOUND('',#1282,.T.);
#990=FACE_OUTER_BOUND('',#1283,.T.);
#991=FACE_OUTER_BOUND('',#1284,.T.);
#992=FACE_OUTER_BOUND('',#1285,.T.);
#993=FACE_OUTER_BOUND('',#1286,.T.);
#994=FACE_OUTER_BOUND('',#1287,.T.);
#995=FACE_OUTER_BOUND('',#1288,.T.);
#996=FACE_OUTER_BOUND('',#1289,.T.);
#997=FACE_OUTER_BOUND('',#1290,.T.);
#998=FACE_OUTER_BOUND('',#1291,.T.);
#999=FACE_OUTER_BOUND('',#1292,.T.);
#1000=FACE_OUTER_BOUND('',#1293,.T.);
#1001=FACE_OUTER_BOUND('',#1294,.T.);
#1002=FACE_OUTER_BOUND('',#1295,.T.);
#1003=FACE_OUTER_BOUND('',#1297,.T.);
#1004=FACE_OUTER_BOUND('',#1299,.T.);
#1005=FACE_OUTER_BOUND('',#1300,.T.);
#1006=FACE_OUTER_BOUND('',#1301,.T.);
#1007=FACE_OUTER_BOUND('',#1302,.T.);
#1008=FACE_OUTER_BOUND('',#1303,.T.);
#1009=FACE_OUTER_BOUND('',#1304,.T.);
#1010=FACE_OUTER_BOUND('',#1305,.T.);
#1011=FACE_OUTER_BOUND('',#1306,.T.);
#1012=FACE_OUTER_BOUND('',#1307,.T.);
#1013=FACE_OUTER_BOUND('',#1308,.T.);
#1014=FACE_OUTER_BOUND('',#1309,.T.);
#1015=FACE_OUTER_BOUND('',#1310,.T.);
#1016=FACE_OUTER_BOUND('',#1311,.T.);
#1017=FACE_OUTER_BOUND('',#1312,.T.);
#1018=FACE_OUTER_BOUND('',#1313,.T.);
#1019=FACE_OUTER_BOUND('',#1314,.T.);
#1020=FACE_OUTER_BOUND('',#1315,.T.);
#1021=FACE_OUTER_BOUND('',#1316,.T.);
#1022=FACE_OUTER_BOUND('',#1317,.T.);
#1023=FACE_OUTER_BOUND('',#1318,.T.);
#1024=FACE_OUTER_BOUND('',#1319,.T.);
#1025=FACE_OUTER_BOUND('',#1320,.T.);
#1026=FACE_OUTER_BOUND('',#1322,.T.);
#1027=FACE_OUTER_BOUND('',#1323,.T.);
#1028=FACE_OUTER_BOUND('',#1324,.T.);
#1029=FACE_OUTER_BOUND('',#1325,.T.);
#1030=FACE_OUTER_BOUND('',#1326,.T.);
#1031=FACE_OUTER_BOUND('',#1327,.T.);
#1032=FACE_OUTER_BOUND('',#1328,.T.);
#1033=EDGE_LOOP('',(#2541,#2542,#2543,#2544,#2545));
#1034=EDGE_LOOP('',(#2546,#2547,#2548,#2549,#2550,#2551,#2552,#2553,#2554,
#2555,#2556,#2557));
#1035=EDGE_LOOP('',(#2558,#2559,#2560,#2561,#2562,#2563,#2564,#2565,#2566));
#1036=EDGE_LOOP('',(#2567,#2568,#2569,#2570,#2571,#2572,#2573));
#1037=EDGE_LOOP('',(#2574));
#1038=EDGE_LOOP('',(#2575));
#1039=EDGE_LOOP('',(#2576));
#1040=EDGE_LOOP('',(#2577));
#1041=EDGE_LOOP('',(#2578));
#1042=EDGE_LOOP('',(#2579,#2580,#2581,#2582,#2583));
#1043=EDGE_LOOP('',(#2584,#2585,#2586,#2587,#2588));
#1044=EDGE_LOOP('',(#2589));
#1045=EDGE_LOOP('',(#2590));
#1046=EDGE_LOOP('',(#2591,#2592,#2593,#2594));
#1047=EDGE_LOOP('',(#2595));
#1048=EDGE_LOOP('',(#2596));
#1049=EDGE_LOOP('',(#2597));
#1050=EDGE_LOOP('',(#2598));
#1051=EDGE_LOOP('',(#2599));
#1052=EDGE_LOOP('',(#2600));
#1053=EDGE_LOOP('',(#2601,#2602,#2603,#2604,#2605));
#1054=EDGE_LOOP('',(#2606));
#1055=EDGE_LOOP('',(#2607));
#1056=EDGE_LOOP('',(#2608));
#1057=EDGE_LOOP('',(#2609));
#1058=EDGE_LOOP('',(#2610));
#1059=EDGE_LOOP('',(#2611));
#1060=EDGE_LOOP('',(#2612,#2613,#2614,#2615,#2616));
#1061=EDGE_LOOP('',(#2617,#2618,#2619,#2620,#2621));
#1062=EDGE_LOOP('',(#2622));
#1063=EDGE_LOOP('',(#2623));
#1064=EDGE_LOOP('',(#2624,#2625,#2626,#2627,#2628,#2629,#2630));
#1065=EDGE_LOOP('',(#2631,#2632,#2633,#2634,#2635,#2636,#2637,#2638,#2639));
#1066=EDGE_LOOP('',(#2640,#2641,#2642,#2643,#2644,#2645,#2646,#2647));
#1067=EDGE_LOOP('',(#2648));
#1068=EDGE_LOOP('',(#2649));
#1069=EDGE_LOOP('',(#2650));
#1070=EDGE_LOOP('',(#2651));
#1071=EDGE_LOOP('',(#2652));
#1072=EDGE_LOOP('',(#2653));
#1073=EDGE_LOOP('',(#2654,#2655,#2656,#2657,#2658));
#1074=EDGE_LOOP('',(#2659));
#1075=EDGE_LOOP('',(#2660));
#1076=EDGE_LOOP('',(#2661,#2662,#2663,#2664));
#1077=EDGE_LOOP('',(#2665,#2666));
#1078=EDGE_LOOP('',(#2667));
#1079=EDGE_LOOP('',(#2668));
#1080=EDGE_LOOP('',(#2669,#2670,#2671,#2672));
#1081=EDGE_LOOP('',(#2673,#2674,#2675,#2676));
#1082=EDGE_LOOP('',(#2677));
#1083=EDGE_LOOP('',(#2678));
#1084=EDGE_LOOP('',(#2679));
#1085=EDGE_LOOP('',(#2680));
#1086=EDGE_LOOP('',(#2681));
#1087=EDGE_LOOP('',(#2682));
#1088=EDGE_LOOP('',(#2683));
#1089=EDGE_LOOP('',(#2684));
#1090=EDGE_LOOP('',(#2685));
#1091=EDGE_LOOP('',(#2686));
#1092=EDGE_LOOP('',(#2687));
#1093=EDGE_LOOP('',(#2688));
#1094=EDGE_LOOP('',(#2689,#2690,#2691,#2692));
#1095=EDGE_LOOP('',(#2693,#2694,#2695,#2696,#2697));
#1096=EDGE_LOOP('',(#2698,#2699,#2700,#2701,#2702));
#1097=EDGE_LOOP('',(#2703,#2704,#2705,#2706,#2707));
#1098=EDGE_LOOP('',(#2708,#2709,#2710,#2711));
#1099=EDGE_LOOP('',(#2712,#2713,#2714,#2715));
#1100=EDGE_LOOP('',(#2716,#2717,#2718,#2719));
#1101=EDGE_LOOP('',(#2720,#2721,#2722,#2723));
#1102=EDGE_LOOP('',(#2724,#2725,#2726,#2727));
#1103=EDGE_LOOP('',(#2728,#2729,#2730,#2731));
#1104=EDGE_LOOP('',(#2732,#2733,#2734,#2735));
#1105=EDGE_LOOP('',(#2736,#2737,#2738,#2739));
#1106=EDGE_LOOP('',(#2740,#2741,#2742,#2743,#2744));
#1107=EDGE_LOOP('',(#2745,#2746,#2747,#2748));
#1108=EDGE_LOOP('',(#2749,#2750,#2751,#2752));
#1109=EDGE_LOOP('',(#2753,#2754,#2755,#2756));
#1110=EDGE_LOOP('',(#2757,#2758,#2759,#2760));
#1111=EDGE_LOOP('',(#2761,#2762,#2763,#2764,#2765));
#1112=EDGE_LOOP('',(#2766,#2767,#2768,#2769,#2770));
#1113=EDGE_LOOP('',(#2771,#2772,#2773,#2774,#2775));
#1114=EDGE_LOOP('',(#2776,#2777,#2778,#2779,#2780));
#1115=EDGE_LOOP('',(#2781,#2782,#2783));
#1116=EDGE_LOOP('',(#2784,#2785,#2786));
#1117=EDGE_LOOP('',(#2787,#2788,#2789));
#1118=EDGE_LOOP('',(#2790,#2791,#2792));
#1119=EDGE_LOOP('',(#2793,#2794,#2795,#2796,#2797));
#1120=EDGE_LOOP('',(#2798,#2799,#2800,#2801,#2802));
#1121=EDGE_LOOP('',(#2803,#2804,#2805,#2806,#2807));
#1122=EDGE_LOOP('',(#2808,#2809,#2810,#2811,#2812));
#1123=EDGE_LOOP('',(#2813));
#1124=EDGE_LOOP('',(#2814));
#1125=EDGE_LOOP('',(#2815,#2816,#2817,#2818,#2819,#2820,#2821,#2822,#2823,
#2824,#2825,#2826));
#1126=EDGE_LOOP('',(#2827));
#1127=EDGE_LOOP('',(#2828,#2829));
#1128=EDGE_LOOP('',(#2830,#2831));
#1129=EDGE_LOOP('',(#2832,#2833,#2834,#2835,#2836));
#1130=EDGE_LOOP('',(#2837,#2838,#2839,#2840,#2841,#2842,#2843,#2844,#2845,
#2846,#2847,#2848,#2849));
#1131=EDGE_LOOP('',(#2850,#2851,#2852,#2853));
#1132=EDGE_LOOP('',(#2854,#2855,#2856,#2857,#2858));
#1133=EDGE_LOOP('',(#2859));
#1134=EDGE_LOOP('',(#2860,#2861,#2862,#2863));
#1135=EDGE_LOOP('',(#2864,#2865,#2866,#2867));
#1136=EDGE_LOOP('',(#2868,#2869,#2870,#2871));
#1137=EDGE_LOOP('',(#2872,#2873,#2874,#2875));
#1138=EDGE_LOOP('',(#2876,#2877,#2878,#2879,#2880,#2881,#2882,#2883,#2884,
#2885,#2886,#2887));
#1139=EDGE_LOOP('',(#2888,#2889,#2890,#2891,#2892));
#1140=EDGE_LOOP('',(#2893,#2894,#2895,#2896,#2897));
#1141=EDGE_LOOP('',(#2898,#2899,#2900,#2901,#2902));
#1142=EDGE_LOOP('',(#2903,#2904,#2905,#2906,#2907));
#1143=EDGE_LOOP('',(#2908,#2909,#2910,#2911,#2912));
#1144=EDGE_LOOP('',(#2913,#2914,#2915,#2916));
#1145=EDGE_LOOP('',(#2917,#2918,#2919,#2920));
#1146=EDGE_LOOP('',(#2921,#2922,#2923,#2924));
#1147=EDGE_LOOP('',(#2925,#2926,#2927,#2928));
#1148=EDGE_LOOP('',(#2929,#2930,#2931,#2932));
#1149=EDGE_LOOP('',(#2933,#2934,#2935));
#1150=EDGE_LOOP('',(#2936,#2937,#2938));
#1151=EDGE_LOOP('',(#2939,#2940,#2941));
#1152=EDGE_LOOP('',(#2942));
#1153=EDGE_LOOP('',(#2943));
#1154=EDGE_LOOP('',(#2944,#2945,#2946,#2947));
#1155=EDGE_LOOP('',(#2948,#2949,#2950,#2951));
#1156=EDGE_LOOP('',(#2952));
#1157=EDGE_LOOP('',(#2953));
#1158=EDGE_LOOP('',(#2954,#2955,#2956,#2957));
#1159=EDGE_LOOP('',(#2958,#2959));
#1160=EDGE_LOOP('',(#2960,#2961));
#1161=EDGE_LOOP('',(#2962,#2963,#2964,#2965,#2966,#2967));
#1162=EDGE_LOOP('',(#2968,#2969,#2970,#2971));
#1163=EDGE_LOOP('',(#2972,#2973,#2974,#2975,#2976));
#1164=EDGE_LOOP('',(#2977,#2978,#2979,#2980,#2981));
#1165=EDGE_LOOP('',(#2982,#2983,#2984,#2985,#2986));
#1166=EDGE_LOOP('',(#2987,#2988,#2989,#2990,#2991));
#1167=EDGE_LOOP('',(#2992,#2993,#2994));
#1168=EDGE_LOOP('',(#2995,#2996,#2997,#2998,#2999,#3000,#3001));
#1169=EDGE_LOOP('',(#3002));
#1170=EDGE_LOOP('',(#3003));
#1171=EDGE_LOOP('',(#3004));
#1172=EDGE_LOOP('',(#3005));
#1173=EDGE_LOOP('',(#3006));
#1174=EDGE_LOOP('',(#3007,#3008,#3009,#3010,#3011,#3012,#3013,#3014,#3015,
#3016));
#1175=EDGE_LOOP('',(#3017,#3018));
#1176=EDGE_LOOP('',(#3019,#3020,#3021,#3022,#3023,#3024,#3025,#3026,#3027,
#3028));
#1177=EDGE_LOOP('',(#3029,#3030));
#1178=EDGE_LOOP('',(#3031,#3032,#3033,#3034,#3035,#3036,#3037,#3038,#3039,
#3040));
#1179=EDGE_LOOP('',(#3041,#3042,#3043,#3044,#3045,#3046));
#1180=EDGE_LOOP('',(#3047,#3048,#3049,#3050));
#1181=EDGE_LOOP('',(#3051));
#1182=EDGE_LOOP('',(#3052));
#1183=EDGE_LOOP('',(#3053));
#1184=EDGE_LOOP('',(#3054));
#1185=EDGE_LOOP('',(#3055,#3056,#3057,#3058,#3059));
#1186=EDGE_LOOP('',(#3060,#3061,#3062,#3063,#3064,#3065));
#1187=EDGE_LOOP('',(#3066,#3067,#3068,#3069,#3070));
#1188=EDGE_LOOP('',(#3071));
#1189=EDGE_LOOP('',(#3072));
#1190=EDGE_LOOP('',(#3073,#3074,#3075,#3076));
#1191=EDGE_LOOP('',(#3077));
#1192=EDGE_LOOP('',(#3078));
#1193=EDGE_LOOP('',(#3079,#3080,#3081,#3082));
#1194=EDGE_LOOP('',(#3083));
#1195=EDGE_LOOP('',(#3084));
#1196=EDGE_LOOP('',(#3085));
#1197=EDGE_LOOP('',(#3086));
#1198=EDGE_LOOP('',(#3087));
#1199=EDGE_LOOP('',(#3088));
#1200=EDGE_LOOP('',(#3089,#3090,#3091,#3092));
#1201=EDGE_LOOP('',(#3093));
#1202=EDGE_LOOP('',(#3094));
#1203=EDGE_LOOP('',(#3095));
#1204=EDGE_LOOP('',(#3096));
#1205=EDGE_LOOP('',(#3097));
#1206=EDGE_LOOP('',(#3098));
#1207=EDGE_LOOP('',(#3099,#3100,#3101,#3102));
#1208=EDGE_LOOP('',(#3103,#3104,#3105,#3106));
#1209=EDGE_LOOP('',(#3107,#3108,#3109,#3110));
#1210=EDGE_LOOP('',(#3111,#3112,#3113,#3114));
#1211=EDGE_LOOP('',(#3115,#3116,#3117,#3118));
#1212=EDGE_LOOP('',(#3119,#3120,#3121,#3122));
#1213=EDGE_LOOP('',(#3123));
#1214=EDGE_LOOP('',(#3124));
#1215=EDGE_LOOP('',(#3125,#3126,#3127,#3128));
#1216=EDGE_LOOP('',(#3129));
#1217=EDGE_LOOP('',(#3130));
#1218=EDGE_LOOP('',(#3131,#3132,#3133,#3134));
#1219=EDGE_LOOP('',(#3135,#3136,#3137,#3138));
#1220=EDGE_LOOP('',(#3139,#3140,#3141,#3142,#3143));
#1221=EDGE_LOOP('',(#3144,#3145,#3146,#3147,#3148));
#1222=EDGE_LOOP('',(#3149,#3150,#3151,#3152,#3153));
#1223=EDGE_LOOP('',(#3154,#3155,#3156,#3157,#3158));
#1224=EDGE_LOOP('',(#3159,#3160,#3161,#3162,#3163));
#1225=EDGE_LOOP('',(#3164,#3165,#3166,#3167,#3168));
#1226=EDGE_LOOP('',(#3169,#3170,#3171,#3172,#3173,#3174));
#1227=EDGE_LOOP('',(#3175));
#1228=EDGE_LOOP('',(#3176,#3177,#3178,#3179));
#1229=EDGE_LOOP('',(#3180));
#1230=EDGE_LOOP('',(#3181));
#1231=EDGE_LOOP('',(#3182,#3183,#3184));
#1232=EDGE_LOOP('',(#3185,#3186,#3187));
#1233=EDGE_LOOP('',(#3188,#3189,#3190));
#1234=EDGE_LOOP('',(#3191,#3192,#3193));
#1235=EDGE_LOOP('',(#3194,#3195,#3196));
#1236=EDGE_LOOP('',(#3197,#3198,#3199));
#1237=EDGE_LOOP('',(#3200));
#1238=EDGE_LOOP('',(#3201));
#1239=EDGE_LOOP('',(#3202,#3203,#3204,#3205,#3206,#3207,#3208,#3209,#3210));
#1240=EDGE_LOOP('',(#3211,#3212,#3213,#3214));
#1241=EDGE_LOOP('',(#3215));
#1242=EDGE_LOOP('',(#3216));
#1243=EDGE_LOOP('',(#3217,#3218,#3219,#3220));
#1244=EDGE_LOOP('',(#3221,#3222,#3223,#3224,#3225,#3226));
#1245=EDGE_LOOP('',(#3227,#3228,#3229,#3230,#3231,#3232));
#1246=EDGE_LOOP('',(#3233,#3234,#3235,#3236,#3237,#3238));
#1247=EDGE_LOOP('',(#3239,#3240,#3241,#3242,#3243,#3244,#3245));
#1248=EDGE_LOOP('',(#3246,#3247,#3248,#3249,#3250,#3251));
#1249=EDGE_LOOP('',(#3252,#3253,#3254,#3255,#3256,#3257,#3258));
#1250=EDGE_LOOP('',(#3259,#3260,#3261,#3262,#3263,#3264));
#1251=EDGE_LOOP('',(#3265,#3266,#3267,#3268,#3269,#3270));
#1252=EDGE_LOOP('',(#3271,#3272,#3273,#3274,#3275,#3276));
#1253=EDGE_LOOP('',(#3277,#3278,#3279,#3280,#3281,#3282));
#1254=EDGE_LOOP('',(#3283,#3284,#3285,#3286,#3287,#3288));
#1255=EDGE_LOOP('',(#3289,#3290,#3291,#3292,#3293,#3294));
#1256=EDGE_LOOP('',(#3295,#3296,#3297,#3298,#3299,#3300));
#1257=EDGE_LOOP('',(#3301,#3302,#3303,#3304,#3305,#3306));
#1258=EDGE_LOOP('',(#3307,#3308,#3309,#3310,#3311,#3312,#3313,#3314,#3315,
#3316,#3317,#3318,#3319,#3320,#3321,#3322,#3323,#3324,#3325,#3326,#3327,
#3328,#3329,#3330,#3331,#3332,#3333,#3334,#3335,#3336,#3337,#3338,#3339,
#3340,#3341,#3342));
#1259=EDGE_LOOP('',(#3343,#3344,#3345,#3346,#3347,#3348));
#1260=EDGE_LOOP('',(#3349,#3350,#3351,#3352,#3353,#3354));
#1261=EDGE_LOOP('',(#3355,#3356,#3357,#3358,#3359,#3360,#3361,#3362,#3363,
#3364,#3365,#3366));
#1262=EDGE_LOOP('',(#3367,#3368,#3369,#3370));
#1263=EDGE_LOOP('',(#3371,#3372,#3373,#3374));
#1264=EDGE_LOOP('',(#3375,#3376,#3377,#3378));
#1265=EDGE_LOOP('',(#3379));
#1266=EDGE_LOOP('',(#3380,#3381,#3382,#3383));
#1267=EDGE_LOOP('',(#3384));
#1268=EDGE_LOOP('',(#3385,#3386,#3387,#3388));
#1269=EDGE_LOOP('',(#3389,#3390,#3391,#3392));
#1270=EDGE_LOOP('',(#3393,#3394,#3395,#3396));
#1271=EDGE_LOOP('',(#3397,#3398,#3399,#3400));
#1272=EDGE_LOOP('',(#3401,#3402,#3403,#3404));
#1273=EDGE_LOOP('',(#3405,#3406,#3407,#3408,#3409));
#1274=EDGE_LOOP('',(#3410,#3411,#3412,#3413));
#1275=EDGE_LOOP('',(#3414,#3415,#3416,#3417,#3418));
#1276=EDGE_LOOP('',(#3419,#3420,#3421,#3422));
#1277=EDGE_LOOP('',(#3423,#3424,#3425,#3426));
#1278=EDGE_LOOP('',(#3427,#3428,#3429,#3430));
#1279=EDGE_LOOP('',(#3431,#3432,#3433,#3434));
#1280=EDGE_LOOP('',(#3435,#3436,#3437,#3438));
#1281=EDGE_LOOP('',(#3439,#3440,#3441,#3442,#3443));
#1282=EDGE_LOOP('',(#3444,#3445,#3446,#3447,#3448));
#1283=EDGE_LOOP('',(#3449,#3450,#3451,#3452,#3453));
#1284=EDGE_LOOP('',(#3454,#3455,#3456,#3457,#3458));
#1285=EDGE_LOOP('',(#3459,#3460,#3461,#3462,#3463));
#1286=EDGE_LOOP('',(#3464,#3465,#3466,#3467,#3468));
#1287=EDGE_LOOP('',(#3469,#3470,#3471,#3472,#3473));
#1288=EDGE_LOOP('',(#3474,#3475,#3476,#3477,#3478));
#1289=EDGE_LOOP('',(#3479,#3480,#3481,#3482,#3483,#3484));
#1290=EDGE_LOOP('',(#3485,#3486,#3487,#3488,#3489,#3490));
#1291=EDGE_LOOP('',(#3491,#3492,#3493,#3494,#3495,#3496));
#1292=EDGE_LOOP('',(#3497,#3498,#3499,#3500,#3501,#3502));
#1293=EDGE_LOOP('',(#3503,#3504,#3505,#3506,#3507,#3508));
#1294=EDGE_LOOP('',(#3509,#3510,#3511,#3512,#3513,#3514));
#1295=EDGE_LOOP('',(#3515,#3516,#3517,#3518,#3519,#3520));
#1296=EDGE_LOOP('',(#3521));
#1297=EDGE_LOOP('',(#3522,#3523,#3524,#3525,#3526,#3527));
#1298=EDGE_LOOP('',(#3528));
#1299=EDGE_LOOP('',(#3529,#3530,#3531,#3532));
#1300=EDGE_LOOP('',(#3533,#3534,#3535));
#1301=EDGE_LOOP('',(#3536,#3537,#3538));
#1302=EDGE_LOOP('',(#3539,#3540,#3541));
#1303=EDGE_LOOP('',(#3542,#3543,#3544));
#1304=EDGE_LOOP('',(#3545,#3546,#3547));
#1305=EDGE_LOOP('',(#3548,#3549,#3550));
#1306=EDGE_LOOP('',(#3551,#3552,#3553));
#1307=EDGE_LOOP('',(#3554,#3555,#3556));
#1308=EDGE_LOOP('',(#3557,#3558,#3559));
#1309=EDGE_LOOP('',(#3560,#3561,#3562));
#1310=EDGE_LOOP('',(#3563,#3564,#3565));
#1311=EDGE_LOOP('',(#3566,#3567,#3568));
#1312=EDGE_LOOP('',(#3569,#3570,#3571,#3572,#3573));
#1313=EDGE_LOOP('',(#3574,#3575,#3576,#3577,#3578));
#1314=EDGE_LOOP('',(#3579,#3580,#3581,#3582,#3583));
#1315=EDGE_LOOP('',(#3584,#3585,#3586,#3587,#3588));
#1316=EDGE_LOOP('',(#3589,#3590,#3591,#3592,#3593));
#1317=EDGE_LOOP('',(#3594,#3595,#3596,#3597,#3598));
#1318=EDGE_LOOP('',(#3599,#3600,#3601,#3602));
#1319=EDGE_LOOP('',(#3603));
#1320=EDGE_LOOP('',(#3604,#3605,#3606,#3607,#3608,#3609));
#1321=EDGE_LOOP('',(#3610));
#1322=EDGE_LOOP('',(#3611,#3612,#3613));
#1323=EDGE_LOOP('',(#3614,#3615,#3616));
#1324=EDGE_LOOP('',(#3617,#3618,#3619));
#1325=EDGE_LOOP('',(#3620,#3621,#3622));
#1326=EDGE_LOOP('',(#3623,#3624,#3625));
#1327=EDGE_LOOP('',(#3626,#3627,#3628));
#1328=EDGE_LOOP('',(#3629,#3630,#3631,#3632,#3633,#3634));
#1329=B_SPLINE_CURVE_WITH_KNOTS('',3,(#5577,#5578,#5579,#5580,#5581,#5582,
#5583,#5584),.UNSPECIFIED.,.F.,.F.,(4,2,2,4),(-1.5505171028707,-1.25408209125058,
0.,0.00304904819120853),.UNSPECIFIED.);
#1330=B_SPLINE_CURVE_WITH_KNOTS('',3,(#5589,#5590,#5591,#5592,#5593,#5594,
#5595,#5596,#5597,#5598),.UNSPECIFIED.,.F.,.F.,(4,2,2,2,4),(4.80501349520982,
5.06951274232393,5.98994668417101,6.94716893318789,6.95166465756746),
 .UNSPECIFIED.);
#1331=B_SPLINE_CURVE_WITH_KNOTS('',3,(#5602,#5603,#5604,#5605,#5606,#5607,
#5608,#5609,#5610,#5611,#5612,#5613,#5614,#5615,#5616,#5617,#5618,#5619,
#5620,#5621,#5622,#5623,#5624,#5625,#5626,#5627,#5628,#5629,#5630,#5631,
#5632,#5633,#5634,#5635),.UNSPECIFIED.,.F.,.F.,(4,2,2,2,2,2,2,2,2,2,2,2,
2,2,2,2,4),(11.9511654991448,12.7026512908879,13.4541370826309,14.205622874374,
14.9571086661171,15.6995186161844,16.4419285662517,17.184338516319,17.9267484663863,
18.6691583423927,19.4115682183991,20.1539780944055,20.8963879704119,21.6478737273813,
22.3993594843507,23.1508452413201,23.9023309982895),.UNSPECIFIED.);
#1332=B_SPLINE_CURVE_WITH_KNOTS('',3,(#5639,#5640,#5641,#5642,#5643,#5644,
#5645,#5646,#5647,#5648,#5649,#5650,#5651,#5652,#5653,#5654,#5655,#5656),
 .UNSPECIFIED.,.F.,.F.,(4,2,2,2,2,2,2,2,4),(15.4947128296219,15.6730696180795,
16.2614804512611,16.8498912844427,17.4383021176243,18.3068888332102,19.1754755487961,
20.0440622643819,20.9126489799678),.UNSPECIFIED.);
#1333=B_SPLINE_CURVE_WITH_KNOTS('',3,(#5658,#5659,#5660,#5661,#5662,#5663,
#5664,#5665,#5666,#5667),.UNSPECIFIED.,.F.,.F.,(4,2,2,2,4),(-6.98864961225109,
-6.53092622927509,-5.80568103754781,-5.08043584582052,-4.62271246284453),
 .UNSPECIFIED.);
#1334=B_SPLINE_CURVE_WITH_KNOTS('',3,(#5669,#5670,#5671,#5672,#5673,#5674,
#5675,#5676,#5677,#5678,#5679,#5680,#5681,#5682,#5683,#5684,#5685,#5686),
 .UNSPECIFIED.,.F.,.F.,(4,2,2,2,2,2,2,2,4),(-5.41793615034587,-5.23957936188825,
-4.65116852870664,-4.06275769552503,-3.47434686234343,-2.60576014675757,
-1.73717343117172,-0.868586715585868,-1.50990331349021E-14),
 .UNSPECIFIED.);
#1335=B_SPLINE_CURVE_WITH_KNOTS('',3,(#5692,#5693,#5694,#5695,#5696,#5697,
#5698,#5699,#5700,#5701,#5702,#5703,#5704,#5705),.UNSPECIFIED.,.F.,.F.,
(4,2,2,2,2,2,4),(0.,0.75148577435623,1.50297154871246,2.25445732306868,
3.00594309742491,3.74835301046176,3.85208753126486),.UNSPECIFIED.);
#1336=B_SPLINE_CURVE_WITH_KNOTS('',3,(#5707,#5708,#5709,#5710,#5711,#5712,
#5713,#5714,#5715,#5716,#5717,#5718,#5719,#5720,#5721,#5722,#5723,#5724,
#5725,#5726,#5727,#5728),.UNSPECIFIED.,.F.,.F.,(4,2,2,2,2,2,2,2,2,2,4),
(1.02020510036039E-13,0.836743409431383,1.52319262533783,1.73458721528613,
1.86686045602122,1.99232796114447,2.16705857121117,2.37875039685339,2.77213838176281,
3.6146168888541,3.63735578863517),.UNSPECIFIED.);
#1337=B_SPLINE_CURVE_WITH_KNOTS('',3,(#5729,#5730,#5731,#5732,#5733,#5734,
#5735,#5736,#5737,#5738,#5739,#5740,#5741,#5742,#5743,#5744,#5745,#5746,
#5747,#5748,#5749,#5750,#5751,#5752,#5753,#5754,#5755,#5756,#5757,#5758,
#5759,#5760,#5761,#5762,#5763,#5764,#5765,#5766,#5767,#5768,#5769,#5770,
#5771,#5772,#5773,#5774),.UNSPECIFIED.,.F.,.F.,(4,2,2,2,2,2,2,2,2,2,2,2,
2,2,2,2,2,2,2,2,2,2,4),(-15.8032530304094,-15.6995185096063,-14.9571085965695,
-14.2056228222133,-13.454137047857,-12.7026512735008,-11.9511654991446,
-11.1996797247884,-10.4481939504321,-9.6967081760759,-8.94522240171967,
-8.20281248868283,-7.46040257564598,-6.71799266260913,-5.97558274957229,
-5.23317283653545,-4.4907629234986,-3.74835301046175,-3.00594309742491,
-2.25445732306868,-1.50297154871245,-0.751485774356227,0.),
 .UNSPECIFIED.);
#1338=B_SPLINE_CURVE_WITH_KNOTS('',3,(#5785,#5786,#5787,#5788,#5789,#5790,
#5791,#5792,#5793,#5794),.UNSPECIFIED.,.F.,.F.,(4,2,2,2,4),(-1.04015949094204,
-0.932657377635769,-0.838016147397311,-0.758953484458178,-0.692999614147385),
 .UNSPECIFIED.);
#1339=B_SPLINE_CURVE_WITH_KNOTS('',3,(#5796,#5797,#5798,#5799,#5800,#5801,
#5802,#5803,#5804,#5805,#5806,#5807,#5808,#5809,#5810,#5811,#5812,#5813,
#5814,#5815,#5816,#5817,#5818,#5819,#5820,#5821,#5822,#5823,#5824,#5825,
#5826,#5827,#5828,#5829,#5830,#5831,#5832,#5833,#5834,#5835,#5836,#5837,
#5838,#5839,#5840,#5841,#5842,#5843,#5844,#5845,#5846,#5847,#5848,#5849,
#5850,#5851,#5852,#5853,#5854,#5855,#5856,#5857,#5858,#5859,#5860,#5861,
#5862,#5863,#5864,#5865,#5866,#5867,#5868,#5869,#5870,#5871,#5872,#5873,
#5874,#5875,#5876,#5877,#5878,#5879,#5880,#5881,#5882,#5883,#5884,#5885,
#5886,#5887,#5888,#5889,#5890,#5891,#5892,#5893,#5894,#5895,#5896,#5897,
#5898,#5899,#5900,#5901,#5902,#5903,#5904,#5905,#5906,#5907,#5908,#5909,
#5910,#5911,#5912,#5913,#5914,#5915,#5916,#5917,#5918,#5919,#5920,#5921,
#5922,#5923,#5924,#5925,#5926,#5927,#5928,#5929,#5930,#5931,#5932,#5933,
#5934,#5935,#5936,#5937,#5938,#5939,#5940,#5941,#5942,#5943,#5944,#5945,
#5946,#5947,#5948,#5949,#5950,#5951,#5952,#5953,#5954,#5955,#5956,#5957,
#5958,#5959,#5960,#5961,#5962,#5963,#5964,#5965,#5966,#5967,#5968,#5969,
#5970,#5971,#5972,#5973,#5974,#5975,#5976,#5977,#5978,#5979),
 .UNSPECIFIED.,.F.,.F.,(4,3,3,3,3,3,3,3,3,3,3,3,3,3,3,3,3,3,3,3,3,3,3,3,
3,3,3,3,3,3,3,3,3,3,3,3,3,3,3,3,3,3,3,3,3,3,3,3,3,3,3,3,3,3,3,3,3,3,3,3,
3,4),(2.72107972055907E-7,0.00178477543725798,0.00262815346851988,0.00401562885331435,
0.00525603482906771,0.00723037697612098,0.00921337722618793,0.0105117975501634,
0.0126012160788207,0.0131396789107112,0.0155870223193016,0.015767560271259,
0.0173527198466303,0.0183954416318069,0.0196367719226344,0.0208775813990201,
0.0210233229923547,0.0236512043529025,0.0255955755957421,0.0262790857134503,
0.0283626428282405,0.0304454519035474,0.031534848434546,0.0338165992760133,
0.0341627297950938,0.0354766704753677,0.036506599524544,0.0367906111556417,
0.0386488000158229,0.0394184925161895,0.0412258034154853,0.0420463738767373,
0.0442437218200704,0.0446742552372851,0.0467464838413529,0.047302136597833,
0.0493898024917242,0.0499300179583808,0.0520165802882478,0.0525578993189286,
0.0544927525372392,0.0551857806794765,0.0561500246532634,0.0564997213597504,
0.0578136620400243,0.060038018841681,0.0604415434005721,0.0624671007693764,
0.0630694247611199,0.0652001506910268,0.0673302255123812,0.0683251874822156,
0.0702926229698116,0.0722499651986351,0.0735809502033112,0.0748948908835851,
0.0762088315638591,0.0779650853238908,0.0788367129244069,0.0809688957796963,
0.0830959029701868,0.0840924756455026),.UNSPECIFIED.);
#1340=B_SPLINE_CURVE_WITH_KNOTS('',3,(#5981,#5982,#5983,#5984,#5985,#5986,
#5987,#5988,#5989,#5990),.UNSPECIFIED.,.F.,.F.,(4,2,2,2,4),(-0.69090250484878,
-0.624714986528312,-0.545652323589179,-0.45101109335072,-0.34350898004445),
 .UNSPECIFIED.);
#1341=B_SPLINE_CURVE_WITH_KNOTS('',3,(#6113,#6114,#6115,#6116,#6117,#6118,
#6119,#6120,#6121,#6122,#6123,#6124,#6125,#6126,#6127,#6128,#6129,#6130,
#6131,#6132,#6133,#6134,#6135,#6136,#6137,#6138,#6139,#6140,#6141,#6142,
#6143,#6144,#6145,#6146),.UNSPECIFIED.,.F.,.F.,(4,2,2,2,2,2,2,2,2,2,2,2,
2,2,2,2,4),(7.41376519068543,7.87807291581701,8.34238064094858,8.80668836608016,
9.27099609121173,9.73340901491583,10.1958219386199,10.658234862324,11.1206477860281,
11.5830607097322,12.0454736334363,12.5078865571404,12.9702994808445,13.4346072059761,
13.8989149311077,14.3632226562393,14.8275303813708),.UNSPECIFIED.);
#1342=B_SPLINE_CURVE_WITH_KNOTS('',3,(#6147,#6148,#6149,#6150,#6151,#6152,
#6153,#6154,#6155,#6156,#6157,#6158,#6159,#6160,#6161,#6162,#6163,#6164,
#6165,#6166,#6167,#6168,#6169,#6170,#6171,#6172,#6173,#6174,#6175,#6176,
#6177,#6178,#6179,#6180),.UNSPECIFIED.,.F.,.F.,(4,2,2,2,2,2,2,2,2,2,2,2,
2,2,2,2,4),(14.8275303813708,15.2918381065024,15.756145831634,16.2204535567656,
16.6847612818971,17.1471742056012,17.6095871293054,18.0720000530095,18.5344129767136,
18.9968259004177,19.4592388241218,19.9216517478259,20.38406467153,20.8483723966616,
21.3126801217931,21.7769878469247,22.2412955720563),.UNSPECIFIED.);
#1343=B_SPLINE_CURVE_WITH_KNOTS('',3,(#6476,#6477,#6478,#6479,#6480,#6481,
#6482,#6483,#6484,#6485,#6486,#6487,#6488,#6489,#6490,#6491,#6492,#6493),
 .UNSPECIFIED.,.F.,.F.,(4,2,2,2,2,2,2,2,4),(0.605474840211907,0.681164486618941,
0.756854133025976,0.832533196671918,0.90821226031786,0.983891323963802,
1.05957038760974,1.13526003401678,1.21094968042381),.UNSPECIFIED.);
#1344=B_SPLINE_CURVE_WITH_KNOTS('',3,(#6494,#6495,#6496,#6497,#6498,#6499,
#6500,#6501,#6502,#6503,#6504,#6505,#6506,#6507,#6508,#6509,#6510,#6511),
 .UNSPECIFIED.,.F.,.F.,(4,2,2,2,2,2,2,2,4),(1.21094968042381,1.28663932683085,
1.36232897323788,1.43800803688382,1.51368710052977,1.58936616417571,1.66504522782165,
1.74073487422869,1.81642452063572),.UNSPECIFIED.);
#1345=B_SPLINE_CURVE_WITH_KNOTS('',3,(#6514,#6515,#6516,#6517,#6518,#6519,
#6520,#6521,#6522,#6523,#6524,#6525,#6526,#6527,#6528,#6529,#6530,#6531),
 .UNSPECIFIED.,.F.,.F.,(4,2,2,2,2,2,2,2,4),(0.605474840211907,0.681164486618941,
0.756854133025976,0.832533196671918,0.90821226031786,0.983891323963802,
1.05957038760974,1.13526003401678,1.21094968042381),.UNSPECIFIED.);
#1346=B_SPLINE_CURVE_WITH_KNOTS('',3,(#6532,#6533,#6534,#6535,#6536,#6537,
#6538,#6539,#6540,#6541,#6542,#6543,#6544,#6545,#6546,#6547,#6548,#6549),
 .UNSPECIFIED.,.F.,.F.,(4,2,2,2,2,2,2,2,4),(1.21094968042381,1.28663932683085,
1.36232897323788,1.43800803688382,1.51368710052977,1.58936616417571,1.66504522782165,
1.74073487422869,1.81642452063572),.UNSPECIFIED.);
#1347=B_SPLINE_CURVE_WITH_KNOTS('',3,(#6587,#6588,#6589,#6590,#6591,#6592,
#6593,#6594),.UNSPECIFIED.,.F.,.F.,(4,2,2,4),(0.904796449630696,0.980250998994914,
1.05570554835913,1.06208648908207),.UNSPECIFIED.);
#1348=B_SPLINE_CURVE_WITH_KNOTS('',3,(#6596,#6597,#6598,#6599,#6600,#6601),
 .UNSPECIFIED.,.F.,.F.,(4,2,4),(-0.144308777092194,-0.0753448589075656,
0.),.UNSPECIFIED.);
#1349=B_SPLINE_CURVE_WITH_KNOTS('',3,(#6603,#6604,#6605,#6606,#6607,#6608,
#6609,#6610,#6611,#6612),.UNSPECIFIED.,.F.,.F.,(4,2,2,2,4),(0.,0.0753448589075656,
0.150689717815131,0.226144267179348,0.301598816543565),.UNSPECIFIED.);
#1350=B_SPLINE_CURVE_WITH_KNOTS('',3,(#6614,#6615,#6616,#6617,#6618,#6619,
#6620,#6621,#6622,#6623,#6624,#6625,#6626,#6627,#6628,#6629,#6630,#6631),
 .UNSPECIFIED.,.F.,.F.,(4,2,2,2,2,2,2,2,4),(0.301598816543565,0.377053365907783,
0.452507915272,0.527852774179565,0.603197633087131,0.678542491994697,0.753887350902262,
0.829341900266479,0.904796449630696),.UNSPECIFIED.);
#1351=B_SPLINE_CURVE_WITH_KNOTS('',3,(#6634,#6635,#6636,#6637,#6638,#6639,
#6640,#6641,#6642,#6643,#6644,#6645,#6646,#6647,#6648,#6649,#6650,#6651,
#6652,#6653,#6654,#6655,#6656,#6657,#6658,#6659,#6660,#6661,#6662,#6663,
#6664,#6665),.UNSPECIFIED.,.F.,.F.,(4,2,2,2,2,2,2,2,2,2,2,2,2,2,2,4),(-0.795209907356727,
-0.792063991439152,-0.735493455630304,-0.678922919821455,-0.622352384012607,
-0.565781848203759,-0.509198564042365,-0.45261527988097,-0.396031995719576,
-0.339448711558182,-0.282878175749333,-0.226307639940485,-0.169737104131637,
-0.113166568322789,-0.0565832841613944,0.),.UNSPECIFIED.);
#1352=B_SPLINE_CURVE_WITH_KNOTS('',3,(#6666,#6667,#6668,#6669,#6670,#6671),
 .UNSPECIFIED.,.F.,.F.,(4,2,4),(0.,0.0565832841613945,0.110020652405213),
 .UNSPECIFIED.);
#1353=B_SPLINE_CURVE_WITH_KNOTS('',3,(#6676,#6677,#6678,#6679,#6680,#6681,
#6682,#6683,#6684,#6685),.UNSPECIFIED.,.F.,.F.,(4,2,2,2,4),(0.,0.0714283614509827,
0.142856722901965,0.214461611703495,0.286066500505024),.UNSPECIFIED.);
#1354=B_SPLINE_CURVE_WITH_KNOTS('',3,(#6687,#6688,#6689,#6690,#6691,#6692),
 .UNSPECIFIED.,.F.,.F.,(4,2,4),(-0.137591291556128,-0.0714283614509829,
0.),.UNSPECIFIED.);
#1355=B_SPLINE_CURVE_WITH_KNOTS('',3,(#6694,#6695,#6696,#6697,#6698,#6699,
#6700,#6701),.UNSPECIFIED.,.F.,.F.,(4,2,2,4),(0.858199501515072,0.929804390316601,
1.00140927911813,1.00667471046397),.UNSPECIFIED.);
#1356=B_SPLINE_CURVE_WITH_KNOTS('',3,(#6703,#6704,#6705,#6706,#6707,#6708,
#6709,#6710,#6711,#6712,#6713,#6714,#6715,#6716,#6717,#6718,#6719,#6720),
 .UNSPECIFIED.,.F.,.F.,(4,2,2,2,2,2,2,2,4),(0.286066500505024,0.357671389306553,
0.429276278108082,0.500704639559065,0.572133001010048,0.64356136246103,
0.714989723912013,0.786594612713542,0.858199501515072),.UNSPECIFIED.);
#1357=B_SPLINE_CURVE_WITH_KNOTS('',3,(#6723,#6724,#6725,#6726,#6727,#6728,
#6729,#6730,#6731,#6732,#6733,#6734,#6735,#6736,#6737,#6738,#6739,#6740,
#6741,#6742,#6743,#6744,#6745,#6746,#6747,#6748,#6749,#6750,#6751,#6752,
#6753,#6754),.UNSPECIFIED.,.F.,.F.,(4,2,2,2,2,2,2,2,2,2,2,2,2,2,2,4),(-0.856704581886595,
-0.85079361436338,-0.790035269749255,-0.72927692513513,-0.668518580521006,
-0.607760235906881,-0.546972426331817,-0.486184616756754,-0.42539680718169,
-0.364608997606626,-0.303850652992501,-0.243092308378377,-0.182333963764252,
-0.121575619150127,-0.0607878095750637,0.),.UNSPECIFIED.);
#1358=B_SPLINE_CURVE_WITH_KNOTS('',3,(#6755,#6756,#6757,#6758,#6759,#6760),
 .UNSPECIFIED.,.F.,.F.,(4,2,4),(0.,0.0607878095750638,0.115664651626913),
 .UNSPECIFIED.);
#1359=B_SPLINE_CURVE_WITH_KNOTS('',3,(#6875,#6876,#6877,#6878,#6879,#6880,
#6881,#6882,#6883,#6884,#6885,#6886,#6887,#6888,#6889,#6890,#6891,#6892,
#6893,#6894,#6895,#6896),.UNSPECIFIED.,.F.,.F.,(4,2,2,2,2,2,2,2,2,2,4),
(-2.09523377758369,-2.02727170738156,-1.95930963717942,-1.86537787624874,
-1.77144611531805,-1.61404940438782,-1.45665269345759,-1.09248952009319,
-0.728326346728794,-0.364163173364397,0.),.UNSPECIFIED.);
#1360=B_SPLINE_CURVE_WITH_KNOTS('',3,(#6898,#6899,#6900,#6901,#6902,#6903,
#6904,#6905,#6906,#6907,#6908,#6909,#6910,#6911,#6912,#6913,#6914,#6915,
#6916,#6917,#6918,#6919),.UNSPECIFIED.,.F.,.F.,(4,2,2,2,2,2,2,2,2,2,4),
(-8.38093511033477,-8.01677193697037,-7.65260876360598,-7.28844559024158,
-6.92428241687718,-6.76688570594695,-6.60948899501672,-6.51555723408603,
-6.42162547315535,-6.35366340295321,-6.28570133275108),.UNSPECIFIED.);
#1361=B_SPLINE_CURVE_WITH_KNOTS('',3,(#6928,#6929,#6930,#6931,#6932,#6933,
#6934,#6935,#6936,#6937,#6938,#6939,#6940,#6941,#6942,#6943,#6944,#6945),
 .UNSPECIFIED.,.F.,.F.,(4,2,2,2,2,2,2,2,4),(-2.1101163324575,-2.02379922393296,
-1.92362324243839,-1.76357162567649,-1.6035200089146,-1.20264000668595,
-0.801760004457301,-0.40088000222865,0.),.UNSPECIFIED.);
#1362=B_SPLINE_CURVE_WITH_KNOTS('',3,(#6946,#6947,#6948,#6949,#6950,#6951,
#6952,#6953,#6954,#6955,#6956,#6957,#6958,#6959,#6960,#6961,#6962,#6963),
 .UNSPECIFIED.,.F.,.F.,(4,2,2,2,2,2,2,2,4),(-8.44046532983,-8.03958532760135,
-7.6387053253727,-7.23782532314405,-6.8369453209154,-6.67689370415351,-6.51684208739162,
-6.41666610589705,-6.3303489973725),.UNSPECIFIED.);
#1363=B_SPLINE_CURVE_WITH_KNOTS('',3,(#6968,#6969,#6970,#6971,#6972,#6973,
#6974,#6975,#6976,#6977,#6978,#6979,#6980,#6981,#6982,#6983,#6984,#6985),
 .UNSPECIFIED.,.F.,.F.,(4,2,2,2,2,2,2,2,4),(-2.1101163324575,-2.02379922393296,
-1.92362324243838,-1.76357162567649,-1.6035200089146,-1.20264000668595,
-0.8017600044573,-0.40088000222865,0.),.UNSPECIFIED.);
#1364=B_SPLINE_CURVE_WITH_KNOTS('',3,(#6986,#6987,#6988,#6989,#6990,#6991,
#6992,#6993,#6994,#6995,#6996,#6997,#6998,#6999,#7000,#7001,#7002,#7003),
 .UNSPECIFIED.,.F.,.F.,(4,2,2,2,2,2,2,2,4),(-8.44046532983,-8.03958532760135,
-7.6387053253727,-7.23782532314405,-6.8369453209154,-6.67689370415351,-6.51684208739162,
-6.41666610589704,-6.3303489973725),.UNSPECIFIED.);
#1365=B_SPLINE_CURVE_WITH_KNOTS('',3,(#7012,#7013,#7014,#7015,#7016,#7017,
#7018,#7019,#7020,#7021,#7022,#7023,#7024,#7025,#7026,#7027,#7028,#7029),
 .UNSPECIFIED.,.F.,.F.,(4,2,2,2,2,2,2,2,4),(-2.11011633245751,-2.02379922393296,
-1.92362324243839,-1.7635716256765,-1.60352000891461,-1.20264000668595,
-0.801760004457303,-0.400880002228651,0.),.UNSPECIFIED.);
#1366=B_SPLINE_CURVE_WITH_KNOTS('',3,(#7030,#7031,#7032,#7033,#7034,#7035,
#7036,#7037,#7038,#7039,#7040,#7041,#7042,#7043,#7044,#7045,#7046,#7047),
 .UNSPECIFIED.,.F.,.F.,(4,2,2,2,2,2,2,2,4),(-8.44046532983002,-8.03958532760137,
-7.63870532537272,-7.23782532314407,-6.83694532091541,-6.67689370415352,
-6.51684208739163,-6.41666610589706,-6.33034899737251),.UNSPECIFIED.);
#1367=B_SPLINE_CURVE_WITH_KNOTS('',3,(#7054,#7055,#7056,#7057,#7058,#7059,
#7060,#7061,#7062,#7063,#7064,#7065,#7066,#7067,#7068,#7069,#7070,#7071),
 .UNSPECIFIED.,.F.,.F.,(4,2,2,2,2,2,2,2,4),(-2.1101163324575,-2.02379922393296,
-1.92362324243838,-1.76357162567649,-1.6035200089146,-1.20264000668595,
-0.801760004457301,-0.40088000222865,0.),.UNSPECIFIED.);
#1368=B_SPLINE_CURVE_WITH_KNOTS('',3,(#7072,#7073,#7074,#7075,#7076,#7077,
#7078,#7079,#7080,#7081,#7082,#7083,#7084,#7085,#7086,#7087,#7088,#7089),
 .UNSPECIFIED.,.F.,.F.,(4,2,2,2,2,2,2,2,4),(-8.44046532983,-8.03958532760135,
-7.6387053253727,-7.23782532314405,-6.8369453209154,-6.67689370415351,-6.51684208739162,
-6.41666610589705,-6.3303489973725),.UNSPECIFIED.);
#1369=B_SPLINE_CURVE_WITH_KNOTS('',3,(#7093,#7094,#7095,#7096,#7097,#7098,
#7099,#7100,#7101,#7102,#7103,#7104,#7105,#7106,#7107,#7108,#7109,#7110),
 .UNSPECIFIED.,.F.,.F.,(4,2,2,2,2,2,2,2,4),(-2.1101163324575,-2.02379922393296,
-1.92362324243838,-1.76357162567649,-1.6035200089146,-1.20264000668595,
-0.8017600044573,-0.40088000222865,0.),.UNSPECIFIED.);
#1370=B_SPLINE_CURVE_WITH_KNOTS('',3,(#7111,#7112,#7113,#7114,#7115,#7116,
#7117,#7118,#7119,#7120,#7121,#7122,#7123,#7124,#7125,#7126,#7127,#7128),
 .UNSPECIFIED.,.F.,.F.,(4,2,2,2,2,2,2,2,4),(-8.44046532983,-8.03958532760135,
-7.6387053253727,-7.23782532314405,-6.8369453209154,-6.67689370415351,-6.51684208739162,
-6.41666610589704,-6.3303489973725),.UNSPECIFIED.);
#1371=B_SPLINE_CURVE_WITH_KNOTS('',3,(#7174,#7175,#7176,#7177,#7178,#7179,
#7180,#7181,#7182,#7183,#7184,#7185,#7186,#7187,#7188,#7189,#7190,#7191,
#7192,#7193,#7194,#7195,#7196,#7197,#7198,#7199,#7200,#7201,#7202,#7203,
#7204,#7205,#7206,#7207,#7208,#7209,#7210,#7211,#7212,#7213,#7214,#7215,
#7216,#7217,#7218,#7219,#7220,#7221,#7222,#7223,#7224,#7225,#7226,#7227,
#7228,#7229,#7230,#7231,#7232,#7233,#7234,#7235,#7236,#7237,#7238,#7239,
#7240,#7241,#7242,#7243,#7244,#7245,#7246,#7247,#7248,#7249,#7250,#7251,
#7252,#7253,#7254,#7255,#7256,#7257,#7258,#7259,#7260,#7261),
 .UNSPECIFIED.,.F.,.F.,(4,3,3,3,3,3,3,3,3,3,3,3,3,3,3,3,3,3,3,3,3,3,3,3,
3,3,3,3,3,4),(0.,0.000406240529099286,0.00137938545876311,0.00157223368396575,
0.00235712040686395,0.00235835052594862,0.0031444673679315,0.00333814638883581,
0.00417473181206057,0.00431968916279243,0.00471670105189724,0.00530146021537391,
0.00628278928089295,0.00628893473586299,0.00698096938738472,0.00707505157784587,
0.00726415374654744,0.00786116841982874,0.00824590532689442,0.00864728526181162,
0.00916646995968722,0.00922701267009175,0.00943340210379449,0.0101214219001075,
0.0102072274047249,0.0108935730580786,0.0110056357877602,0.0120607068335696,
0.0121610933723902,0.012577869471726),.UNSPECIFIED.);
#1372=B_SPLINE_CURVE_WITH_KNOTS('',3,(#7265,#7266,#7267,#7268,#7269,#7270,
#7271,#7272,#7273,#7274),.UNSPECIFIED.,.F.,.F.,(4,2,2,2,4),(-0.917009726243287,
-0.836713680249397,-0.758350426571219,-0.683089589535854,-0.610699399852799),
 .UNSPECIFIED.);
#1373=B_SPLINE_CURVE_WITH_KNOTS('',3,(#7277,#7278,#7279,#7280,#7281,#7282,
#7283,#7284,#7285,#7286),.UNSPECIFIED.,.F.,.F.,(4,2,2,2,4),(-0.610699399852799,
-0.538309210169743,-0.463048373134379,-0.384685119456201,-0.30438907346231),
 .UNSPECIFIED.);
#1374=B_SPLINE_CURVE_WITH_KNOTS('',3,(#7292,#7293,#7294,#7295,#7296,#7297,
#7298,#7299,#7300,#7301,#7302,#7303,#7304,#7305,#7306,#7307,#7308,#7309,
#7310,#7311,#7312,#7313,#7314,#7315,#7316,#7317,#7318,#7319,#7320,#7321,
#7322,#7323,#7324,#7325,#7326,#7327,#7328,#7329,#7330,#7331,#7332,#7333,
#7334,#7335,#7336,#7337,#7338,#7339,#7340,#7341,#7342,#7343,#7344,#7345,
#7346,#7347,#7348,#7349,#7350,#7351,#7352,#7353,#7354,#7355,#7356,#7357,
#7358,#7359,#7360,#7361,#7362,#7363,#7364,#7365,#7366,#7367,#7368,#7369,
#7370,#7371,#7372,#7373,#7374,#7375,#7376,#7377,#7378,#7379,#7380,#7381,
#7382),.UNSPECIFIED.,.F.,.F.,(4,3,3,3,3,3,3,3,3,3,3,3,3,3,3,3,3,3,3,3,3,
3,3,3,3,3,3,3,3,3,4),(2.60208521396521E-18,0.000400192674595473,0.00127218628897403,
0.00137785726958694,0.00157876092999531,0.00227142090955615,0.0023618191099302,
0.00236814139499296,0.00315752185999062,0.00334675544179567,0.0043315650279144,
0.00473628278998593,0.00531664189634561,0.00552566325498358,0.0061211332819969,
0.00630145520527624,0.00631504371998124,0.00698165466480908,0.00728672101907334,
0.00789380464997654,0.00827095042480516,0.0086831851149742,0.00918475578885096,
0.00925631171880029,0.00947256557997185,0.0102418473576122,0.0110513265099672,
0.0112276216640443,0.0118264377408911,0.0122140928457701,0.0126300874399625),
 .UNSPECIFIED.);
#1375=B_SPLINE_CURVE_WITH_KNOTS('',3,(#7386,#7387,#7388,#7389,#7390,#7391,
#7392,#7393,#7394,#7395),.UNSPECIFIED.,.F.,.F.,(4,2,2,2,4),(0.30438907346231,
0.384685119456201,0.463048373134379,0.538309210169743,0.610699399852799),
 .UNSPECIFIED.);
#1376=B_SPLINE_CURVE_WITH_KNOTS('',3,(#7398,#7399,#7400,#7401,#7402,#7403,
#7404,#7405,#7406,#7407),.UNSPECIFIED.,.F.,.F.,(4,2,2,2,4),(0.610699399852799,
0.683089589535854,0.758350426571219,0.836713680249397,0.917009726243287),
 .UNSPECIFIED.);
#1377=B_SPLINE_CURVE_WITH_KNOTS('',3,(#7411,#7412,#7413,#7414,#7415,#7416,
#7417,#7418,#7419,#7420,#7421,#7422),.UNSPECIFIED.,.F.,.F.,(4,2,2,2,2,4),
(-0.362882917350416,-0.274135453989767,-0.182717407796491,-0.100687086335371,
-0.0480780172014038,0.),.UNSPECIFIED.);
#1378=B_SPLINE_CURVE_WITH_KNOTS('',3,(#7425,#7426,#7427,#7428,#7429,#7430,
#7431,#7432,#7433,#7434,#7435,#7436),.UNSPECIFIED.,.F.,.F.,(4,2,2,2,2,4),
(-0.365096706754078,-0.31691860503495,-0.264216176140628,-0.181784514384503,
-0.0898745758923246,-9.99999994033989E-7),.UNSPECIFIED.);
#1379=B_SPLINE_CURVE_WITH_KNOTS('',3,(#7446,#7447,#7448,#7449,#7450,#7451,
#7452,#7453,#7454,#7455,#7456,#7457),.UNSPECIFIED.,.F.,.F.,(4,2,2,2,2,4),
(-0.362876736231209,-0.274133802851703,-0.182716474898388,-0.100684866470481,
-0.0480764814879336,0.),.UNSPECIFIED.);
#1380=B_SPLINE_CURVE_WITH_KNOTS('',3,(#7462,#7463,#7464,#7465,#7466,#7467,
#7468,#7469,#7470,#7471,#7472,#7473),.UNSPECIFIED.,.F.,.F.,(4,2,2,2,2,4),
(-0.365091922937845,-0.316913549080402,-0.26421121051335,-0.181781618094101,
-0.089862766267777,-9.99999992201683E-7),.UNSPECIFIED.);
#1381=B_SPLINE_CURVE_WITH_KNOTS('',3,(#7483,#7484,#7485,#7486,#7487,#7488,
#7489,#7490,#7491,#7492,#7493,#7494),.UNSPECIFIED.,.F.,.F.,(4,2,2,2,2,4),
(-0.362882338171715,-0.274127578782018,-0.182717811491084,-0.100689968817147,
-0.0480792415446598,0.),.UNSPECIFIED.);
#1382=B_SPLINE_CURVE_WITH_KNOTS('',3,(#7497,#7498,#7499,#7500,#7501,#7502,
#7503,#7504,#7505,#7506,#7507,#7508),.UNSPECIFIED.,.F.,.F.,(4,2,2,2,2,4),
(-0.365095174259356,-0.316917006202739,-0.264214779903918,-0.181783926909875,
-0.0898710353312815,-9.99999992257194E-7),.UNSPECIFIED.);
#1383=B_SPLINE_CURVE_WITH_KNOTS('',3,(#7518,#7519,#7520,#7521,#7522,#7523,
#7524,#7525,#7526,#7527,#7528,#7529),.UNSPECIFIED.,.F.,.F.,(4,2,2,2,2,4),
(-0.362869289557713,-0.274152784534485,-0.182713567211171,-0.100681309588015,
-0.0480754657457727,-6.35607511623171E-8),.UNSPECIFIED.);
#1384=B_SPLINE_CURVE_WITH_KNOTS('',3,(#7534,#7535,#7536,#7537,#7538,#7539,
#7540,#7541,#7542,#7543,#7544,#7545),.UNSPECIFIED.,.F.,.F.,(4,2,2,2,2,4),
(-0.365071317763414,-0.316894297426638,-0.264193403878945,-0.181773042602845,
-0.0898848198288387,0.),.UNSPECIFIED.);
#1385=B_SPLINE_CURVE_WITH_KNOTS('',3,(#7549,#7550,#7551,#7552,#7553,#7554,
#7555,#7556,#7557,#7558,#7559,#7560),.UNSPECIFIED.,.F.,.F.,(4,2,2,2,2,4),
(-0.362871505646336,-0.274155479863949,-0.18271451894341,-0.100676077089741,
-0.0480731533577358,-4.69376613687622E-8),.UNSPECIFIED.);
#1386=B_SPLINE_CURVE_WITH_KNOTS('',3,(#7563,#7564,#7565,#7566,#7567,#7568,
#7569,#7570,#7571,#7572,#7573,#7574),.UNSPECIFIED.,.F.,.F.,(4,2,2,2,2,4),
(-0.365098439792926,-0.316918710131062,-0.264213937899729,-0.181785743458761,
-0.0898914967914955,-9.99999990813905E-7),.UNSPECIFIED.);
#1387=B_SPLINE_CURVE_WITH_KNOTS('',3,(#7584,#7585,#7586,#7587,#7588,#7589,
#7590,#7591,#7592,#7593,#7594,#7595),.UNSPECIFIED.,.F.,.F.,(4,2,2,2,2,4),
(-0.362884032462414,-0.274132691310732,-0.182717829525349,-0.100688494943236,
-0.0480786317165661,0.),.UNSPECIFIED.);
#1388=B_SPLINE_CURVE_WITH_KNOTS('',3,(#7598,#7599,#7600,#7601,#7602,#7603,
#7604,#7605,#7606,#7607,#7608,#7609),.UNSPECIFIED.,.F.,.F.,(4,2,2,2,2,4),
(-0.365096305665182,-0.31691825532505,-0.264216003972505,-0.181784730484854,
-0.0898741884806459,-9.99999991813105E-7),.UNSPECIFIED.);
#1389=B_SPLINE_CURVE_WITH_KNOTS('',3,(#7612,#7613,#7614,#7615,#7616,#7617,
#7618,#7619,#7620,#7621,#7622,#7623,#7624,#7625,#7626,#7627,#7628,#7629,
#7630,#7631,#7632,#7633,#7634,#7635,#7636,#7637,#7638,#7639,#7640,#7641,
#7642,#7643,#7644,#7645,#7646,#7647,#7648,#7649,#7650,#7651,#7652,#7653,
#7654,#7655,#7656,#7657,#7658,#7659,#7660,#7661,#7662,#7663,#7664,#7665,
#7666,#7667,#7668,#7669,#7670,#7671,#7672,#7673,#7674,#7675,#7676,#7677,
#7678,#7679,#7680,#7681,#7682,#7683,#7684,#7685,#7686,#7687,#7688,#7689,
#7690,#7691,#7692,#7693,#7694,#7695,#7696,#7697,#7698,#7699),
 .UNSPECIFIED.,.F.,.F.,(4,3,3,3,3,3,3,3,3,3,3,3,3,3,3,3,3,3,3,3,3,3,3,3,
3,3,3,3,3,4),(1.38777878078145E-17,0.000399606416623122,0.00129850035904466,
0.00137933684600951,0.00158113969895516,0.00218306995011964,0.00236541975885409,
0.00237170954843273,0.0031622793979103,0.00420324675762938,0.00433750131101735,
0.00474341909686545,0.00532262963062005,0.0060793421404212,0.00630880058678835,
0.00632455879582059,0.00729497563368212,0.00790569849477573,0.00828085431408244,
0.00869626834425331,0.00921480780263691,0.00926713505608969,0.00948683819373088,
0.0102553852467388,0.0109880837570885,0.011067977892686,0.0112448745518984,
0.0117403235766751,0.0122357726014517,0.0126491175916412),.UNSPECIFIED.);
#1390=B_SPLINE_CURVE_WITH_KNOTS('',3,(#7703,#7704,#7705,#7706,#7707,#7708,
#7709,#7710,#7711,#7712),.UNSPECIFIED.,.F.,.F.,(4,2,2,2,4),(-0.917009726243287,
-0.836713680249397,-0.758350426571219,-0.683089589535854,-0.610699399852799),
 .UNSPECIFIED.);
#1391=B_SPLINE_CURVE_WITH_KNOTS('',3,(#7715,#7716,#7717,#7718,#7719,#7720,
#7721,#7722,#7723,#7724),.UNSPECIFIED.,.F.,.F.,(4,2,2,2,4),(-0.610699399852799,
-0.538309210169743,-0.463048373134379,-0.384685119456201,-0.30438907346231),
 .UNSPECIFIED.);
#1392=B_SPLINE_CURVE_WITH_KNOTS('',3,(#7729,#7730,#7731,#7732,#7733,#7734,
#7735,#7736,#7737,#7738,#7739,#7740,#7741,#7742,#7743,#7744,#7745,#7746,
#7747,#7748,#7749,#7750,#7751,#7752,#7753,#7754,#7755,#7756,#7757,#7758,
#7759,#7760,#7761,#7762,#7763,#7764,#7765,#7766,#7767,#7768,#7769,#7770,
#7771,#7772,#7773,#7774,#7775,#7776,#7777,#7778,#7779,#7780,#7781,#7782,
#7783,#7784,#7785,#7786,#7787,#7788,#7789,#7790,#7791,#7792,#7793,#7794,
#7795,#7796,#7797,#7798,#7799,#7800,#7801,#7802,#7803,#7804,#7805,#7806,
#7807,#7808,#7809,#7810),.UNSPECIFIED.,.F.,.F.,(4,3,3,3,3,3,3,3,3,3,3,3,
3,3,3,3,3,3,3,3,3,3,3,3,3,3,3,4),(2.60208521396521E-18,0.000408621230909919,
0.00138092877422375,0.00156984971266035,0.00235477456899053,0.00235698685553903,
0.0031396994253207,0.00333641997351489,0.00420225476883832,0.00431638805279074,
0.00470954913798105,0.00529643442975242,0.00627638074485589,0.0062793988506414,
0.00706432370697158,0.00725654782189099,0.00784924856330175,0.00823639758948238,
0.00863417341963193,0.0092162185048964,0.0094190982759621,0.01003718926061,
0.0101955027955133,0.0102040231322923,0.0109889479886225,0.0111714628099954,
0.0121441014440987,0.0125587977012828),.UNSPECIFIED.);
#1393=B_SPLINE_CURVE_WITH_KNOTS('',3,(#7812,#7813,#7814,#7815,#7816,#7817,
#7818,#7819,#7820,#7821),.UNSPECIFIED.,.F.,.F.,(4,2,2,2,4),(0.30438907346231,
0.384685119456201,0.463048373134379,0.538309210169743,0.610699399852799),
 .UNSPECIFIED.);
#1394=B_SPLINE_CURVE_WITH_KNOTS('',3,(#7824,#7825,#7826,#7827,#7828,#7829,
#7830,#7831,#7832,#7833),.UNSPECIFIED.,.F.,.F.,(4,2,2,2,4),(0.610699399852799,
0.683089589535854,0.758350426571219,0.836713680249397,0.917009726243287),
 .UNSPECIFIED.);
#1395=B_SPLINE_CURVE_WITH_KNOTS('',3,(#7835,#7836,#7837,#7838,#7839,#7840,
#7841,#7842,#7843,#7844,#7845,#7846,#7847,#7848,#7849,#7850,#7851,#7852,
#7853,#7854,#7855,#7856,#7857,#7858,#7859,#7860,#7861,#7862,#7863,#7864,
#7865,#7866,#7867,#7868,#7869,#7870,#7871,#7872,#7873,#7874,#7875,#7876,
#7877,#7878,#7879,#7880,#7881,#7882,#7883,#7884,#7885,#7886,#7887,#7888,
#7889,#7890,#7891,#7892,#7893,#7894,#7895,#7896,#7897,#7898,#7899,#7900,
#7901,#7902,#7903,#7904,#7905,#7906,#7907,#7908,#7909,#7910,#7911,#7912,
#7913,#7914,#7915,#7916,#7917,#7918,#7919),.UNSPECIFIED.,.F.,.F.,(4,3,3,
3,3,3,3,3,3,3,3,3,3,3,3,3,3,3,3,3,3,3,3,3,3,3,3,3,4),(1.30496590065728E-17,
0.000400535898609883,0.000997223897656586,0.00138427158256107,0.00158086386747061,
0.00237117917706769,0.00316172773494121,0.00390531090957887,0.00434542243932705,
0.00474259160241181,0.00524658086419516,0.00533175204143861,0.00553302353614712,
0.00610814380124694,0.00631869508804951,0.00632345546988242,0.00711388740361772,
0.00730535224261997,0.00790431933735302,0.00829245922415217,0.00869475127108832,
0.00927921238445572,0.00948518320482362,0.0102661645794107,0.0110660470722942,
0.0112527819469325,0.0117750630618308,0.0122387403294437,0.0126469109397648),
 .UNSPECIFIED.);
#1396=B_SPLINE_CURVE_WITH_KNOTS('',3,(#7921,#7922,#7923,#7924,#7925,#7926,
#7927,#7928,#7929,#7930),.UNSPECIFIED.,.F.,.F.,(4,2,2,2,4),(-0.917010857974424,
-0.836714811980533,-0.758351558302355,-0.683090721266991,-0.610700531583935),
 .UNSPECIFIED.);
#1397=B_SPLINE_CURVE_WITH_KNOTS('',3,(#7933,#7934,#7935,#7936,#7937,#7938,
#7939,#7940,#7941,#7942),.UNSPECIFIED.,.F.,.F.,(4,2,2,2,4),(-0.610699399852799,
-0.538309210169743,-0.463048373134379,-0.384685119456201,-0.30438907346231),
 .UNSPECIFIED.);
#1398=B_SPLINE_CURVE_WITH_KNOTS('',3,(#7944,#7945,#7946,#7947,#7948,#7949,
#7950,#7951,#7952,#7953,#7954,#7955,#7956,#7957,#7958,#7959,#7960,#7961,
#7962,#7963,#7964,#7965,#7966,#7967,#7968,#7969,#7970,#7971,#7972,#7973,
#7974,#7975,#7976,#7977,#7978,#7979,#7980,#7981,#7982,#7983,#7984,#7985,
#7986,#7987,#7988,#7989,#7990,#7991,#7992,#7993,#7994,#7995,#7996,#7997,
#7998,#7999,#8000,#8001,#8002,#8003,#8004,#8005,#8006,#8007,#8008,#8009,
#8010,#8011,#8012,#8013,#8014,#8015,#8016,#8017,#8018,#8019,#8020,#8021,
#8022,#8023,#8024,#8025,#8026,#8027,#8028,#8029,#8030,#8031),
 .UNSPECIFIED.,.F.,.F.,(4,3,3,3,3,3,3,3,3,3,3,3,3,3,3,3,3,3,3,3,3,3,3,3,
3,3,3,3,3,4),(3.46944695195361E-18,0.000410051165251199,0.00133968420328458,
0.00156655532439467,0.00221186581193398,0.00235693864354504,0.00300597240703075,
0.00313311064878935,0.00360729264710897,0.00391638831098668,0.00431136042835414,
0.00469966597318402,0.00540563368882195,0.00610076794994382,0.00626622129757869,
0.00626747608388259,0.00681315808315167,0.00704949895977602,0.00724549920617735,
0.00775072389761868,0.00783277662197336,0.00822300176904177,0.00920143005432391,
0.00939933194636803,0.010179032653128,0.0101826096085654,0.0109658872707627,
0.0111531106855899,0.0121225856750134,0.0125324425951574),.UNSPECIFIED.);
#1399=B_SPLINE_CURVE_WITH_KNOTS('',3,(#8033,#8034,#8035,#8036,#8037,#8038,
#8039,#8040,#8041,#8042),.UNSPECIFIED.,.F.,.F.,(4,2,2,2,4),(0.30438907346231,
0.384685119456201,0.463048373134379,0.538309210169743,0.610699399852799),
 .UNSPECIFIED.);
#1400=B_SPLINE_CURVE_WITH_KNOTS('',3,(#8045,#8046,#8047,#8048,#8049,#8050,
#8051,#8052,#8053,#8054),.UNSPECIFIED.,.F.,.F.,(4,2,2,2,4),(0.610699399852799,
0.683089589535855,0.758350426571219,0.836713680249397,0.917009726243288),
 .UNSPECIFIED.);
#1401=B_SPLINE_CURVE_WITH_KNOTS('',3,(#8057,#8058,#8059,#8060,#8061,#8062,
#8063,#8064,#8065,#8066,#8067,#8068,#8069,#8070,#8071,#8072,#8073,#8074,
#8075,#8076,#8077,#8078,#8079,#8080,#8081,#8082,#8083,#8084,#8085,#8086,
#8087,#8088,#8089,#8090,#8091,#8092,#8093,#8094,#8095,#8096,#8097,#8098,
#8099,#8100,#8101,#8102,#8103,#8104,#8105,#8106,#8107,#8108,#8109,#8110,
#8111,#8112,#8113,#8114,#8115,#8116,#8117,#8118,#8119,#8120,#8121,#8122,
#8123,#8124,#8125,#8126,#8127,#8128,#8129,#8130,#8131,#8132,#8133,#8134,
#8135,#8136,#8137,#8138,#8139,#8140,#8141,#8142,#8143,#8144,#8145,#8146,
#8147),.UNSPECIFIED.,.F.,.F.,(4,3,3,3,3,3,3,3,3,3,3,3,3,3,3,3,3,3,3,3,3,
3,3,3,3,3,3,3,3,3,4),(1.73472347597681E-18,0.00039988746592532,0.00129491695484595,
0.00137824963045728,0.00157959224294063,0.00221817566303284,0.00236299587550376,
0.00236938836441095,0.00315918448588126,0.00334829919727405,0.00433350078435649,
0.00473877672882189,0.00531878197917401,0.00552857285029221,0.00621168871910692,
0.00630402471854614,0.00631836897176252,0.00700327686816661,0.00728961045190966,
0.00789796121470315,0.00827440785064211,0.00868775733617347,0.0091828676285263,
0.00926005766828055,0.00947755345764378,0.0102465428671901,0.0110571457005844,
0.0112335337469168,0.0117819684897293,0.0122215199127025,0.012636737943525),
 .UNSPECIFIED.);
#1402=B_SPLINE_CURVE_WITH_KNOTS('',3,(#8151,#8152,#8153,#8154,#8155,#8156,
#8157,#8158,#8159,#8160),.UNSPECIFIED.,.F.,.F.,(4,2,2,2,4),(-0.917009726243287,
-0.836713680249397,-0.758350426571219,-0.683089589535854,-0.610699399852799),
 .UNSPECIFIED.);
#1403=B_SPLINE_CURVE_WITH_KNOTS('',3,(#8163,#8164,#8165,#8166,#8167,#8168,
#8169,#8170,#8171,#8172),.UNSPECIFIED.,.F.,.F.,(4,2,2,2,4),(-0.610699399852799,
-0.538309210169743,-0.463048373134379,-0.384685119456201,-0.30438907346231),
 .UNSPECIFIED.);
#1404=B_SPLINE_CURVE_WITH_KNOTS('',3,(#8177,#8178,#8179,#8180,#8181,#8182,
#8183,#8184,#8185,#8186,#8187,#8188,#8189,#8190,#8191,#8192,#8193,#8194,
#8195,#8196,#8197,#8198,#8199,#8200,#8201,#8202,#8203,#8204,#8205,#8206,
#8207,#8208,#8209,#8210,#8211,#8212,#8213,#8214,#8215,#8216,#8217,#8218,
#8219,#8220,#8221,#8222,#8223,#8224,#8225,#8226,#8227,#8228,#8229,#8230,
#8231,#8232,#8233,#8234,#8235,#8236,#8237,#8238,#8239,#8240,#8241,#8242,
#8243,#8244,#8245,#8246,#8247,#8248,#8249,#8250,#8251,#8252,#8253,#8254,
#8255,#8256,#8257,#8258,#8259,#8260,#8261),.UNSPECIFIED.,.F.,.F.,(4,3,3,
3,3,3,3,3,3,3,3,3,3,3,3,3,3,3,3,3,3,3,3,3,3,3,3,3,4),(6.07153216591882E-18,
0.00040720230965342,0.00137997790341395,0.00157140084496842,0.0023570743820119,
0.00235710126745262,0.00314280168993683,0.00333751194950876,0.00416238965998517,
0.00431851263176076,0.00471420253490524,0.00529977060133669,0.0062805746484409,
0.00628560337987365,0.00707130380235786,0.00726149881588422,0.00785700422484207,
0.00824263329795796,0.00864270464732627,0.00917430501847767,0.00922314347734942,
0.00942840506981048,0.00998906064805868,0.0102032494512671,0.0102141054922947,
0.0109998059147789,0.0119266401717515,0.0121550490383017,0.0125712067597473),
 .UNSPECIFIED.);
#1405=B_SPLINE_CURVE_WITH_KNOTS('',3,(#8263,#8264,#8265,#8266,#8267,#8268,
#8269,#8270,#8271,#8272),.UNSPECIFIED.,.F.,.F.,(4,2,2,2,4),(0.30438907346231,
0.384685119456201,0.463048373134379,0.538309210169743,0.610699399852799),
 .UNSPECIFIED.);
#1406=B_SPLINE_CURVE_WITH_KNOTS('',3,(#8275,#8276,#8277,#8278,#8279,#8280,
#8281,#8282,#8283,#8284),.UNSPECIFIED.,.F.,.F.,(4,2,2,2,4),(0.610699399852799,
0.683089589535855,0.758350426571219,0.836713680249397,0.917009726243288),
 .UNSPECIFIED.);
#1407=B_SPLINE_CURVE_WITH_KNOTS('',3,(#8288,#8289,#8290,#8291,#8292,#8293,
#8294,#8295,#8296,#8297),.UNSPECIFIED.,.F.,.F.,(4,1,1,1,1,1,1,4),(1.30100171735751E-9,
0.0016146554249922,0.00242198313748831,0.00322931084998441,0.00403663856248051,
0.00484396627497661,0.00565129398747271,0.00645802980103412),
 .UNSPECIFIED.);
#1408=B_SPLINE_CURVE_WITH_KNOTS('',3,(#8301,#8302,#8303,#8304,#8305,#8306,
#8307,#8308,#8309,#8310,#8311,#8312,#8313,#8314,#8315,#8316,#8317,#8318,
#8319,#8320,#8321,#8322,#8323,#8324,#8325,#8326,#8327,#8328,#8329,#8330,
#8331,#8332,#8333,#8334,#8335,#8336,#8337,#8338,#8339,#8340,#8341,#8342,
#8343,#8344,#8345,#8346,#8347,#8348,#8349,#8350,#8351,#8352),
 .UNSPECIFIED.,.F.,.F.,(4,3,3,3,3,3,3,3,3,3,3,3,3,3,3,3,3,4),(0.00648543634797121,
0.0064967267157505,0.00649946849415933,0.00731190205592925,0.00731946089640744,
0.00812433561769917,0.00814225039785811,0.00893676917946909,0.00896508534539126,
0.009749202741239,0.00978815035523349,0.010612333053574,0.0113740698647788,
0.0114378447184054,0.0119000363007037,0.0122657233205253,0.0127116726794121,
0.0129989369883187),.UNSPECIFIED.);
#1409=B_SPLINE_CURVE_WITH_KNOTS('',3,(#8356,#8357,#8358,#8359,#8360,#8361,
#8362,#8363,#8364,#8365,#8366),.UNSPECIFIED.,.F.,.F.,(4,1,1,1,1,1,1,1,4),
(6.42162746646723E-10,0.000808623423577319,0.00161724684715464,0.00242587027073195,
0.00323449369430927,0.00404311711788659,0.00485174054146391,0.00566036396504123,
0.00646652117894175),.UNSPECIFIED.);
#1410=B_SPLINE_CURVE_WITH_KNOTS('',3,(#8369,#8370,#8371,#8372,#8373,#8374,
#8375,#8376,#8377,#8378,#8379,#8380,#8381,#8382,#8383,#8384,#8385,#8386,
#8387,#8388,#8389,#8390,#8391,#8392,#8393,#8394,#8395,#8396,#8397,#8398,
#8399,#8400,#8401,#8402,#8403,#8404,#8405,#8406,#8407,#8408,#8409,#8410,
#8411,#8412,#8413,#8414,#8415,#8416,#8417,#8418,#8419,#8420,#8421,#8422,
#8423),.UNSPECIFIED.,.F.,.F.,(4,3,3,3,3,3,3,3,3,3,3,3,3,3,3,3,3,3,4),(0.00647004505939142,
0.00647363968946843,0.00647720040263265,0.00728284465065198,0.00729848964174994,
0.00801241832704487,0.00809204961183553,0.00811990123016667,0.00894157646616379,
0.00971045953420264,0.00976287368659868,0.010321243105252,0.0105196644953862,
0.0105845039445962,0.011274043522722,0.0113288694565697,0.0114042476736799,
0.0124870589427851,0.0129472785059492),.UNSPECIFIED.);
#1411=B_SPLINE_CURVE_WITH_KNOTS('',3,(#8425,#8426,#8427,#8428,#8429,#8430,
#8431,#8432,#8433,#8434),.UNSPECIFIED.,.F.,.F.,(4,1,1,1,1,1,1,4),(0.,0.000811969399540441,
0.00162393879908088,0.00324787759816176,0.0040598469977022,0.00487181639724265,
0.00568378579678309,0.00648320241242164),.UNSPECIFIED.);
#1412=B_SPLINE_CURVE_WITH_KNOTS('',3,(#8437,#8438,#8439,#8440,#8441,#8442,
#8443,#8444,#8445,#8446,#8447,#8448,#8449,#8450,#8451,#8452,#8453,#8454,
#8455,#8456,#8457,#8458,#8459,#8460,#8461,#8462,#8463,#8464,#8465,#8466,
#8467,#8468,#8469,#8470,#8471,#8472,#8473,#8474,#8475,#8476,#8477,#8478,
#8479,#8480,#8481,#8482,#8483,#8484,#8485,#8486,#8487,#8488,#8489,#8490,
#8491,#8492,#8493,#8494),.UNSPECIFIED.,.F.,.F.,(4,3,3,3,3,3,3,3,3,3,3,3,
3,3,3,3,3,3,3,4),(0.00648198680776405,0.0064936104430031,0.00649369947494339,
0.00730541190931131,0.00731614940961611,0.00811712434367923,0.00813876531642026,
0.00892883677804716,0.00896138011049144,0.00974054921241508,0.00978423042042142,
0.010486564667016,0.010552261646783,0.0106072334779918,0.0113639740811509,
0.0114307075734888,0.011991699677843,0.012255239290347,0.012808829510336,
0.0129873989498868),.UNSPECIFIED.);
#1413=B_SPLINE_CURVE_WITH_KNOTS('',3,(#8496,#8497,#8498,#8499,#8500,#8501,
#8502,#8503,#8504,#8505,#8506,#8507,#8508,#8509,#8510,#8511,#8512,#8513,
#8514,#8515,#8516,#8517,#8518,#8519,#8520,#8521,#8522,#8523,#8524,#8525,
#8526,#8527,#8528,#8529,#8530,#8531,#8532,#8533,#8534,#8535,#8536,#8537,
#8538),.UNSPECIFIED.,.F.,.F.,(4,3,3,3,3,3,3,3,3,3,3,3,3,3,4),(9.63404319765764E-10,
0.000487198195571319,0.000809509611833977,0.00122696048983144,0.00161901922366795,
0.00219920987370979,0.00278322336955574,0.00323803844733591,0.00371315641008233,
0.00404754805916988,0.00445496587286083,0.00485705767100386,0.0055156033353318,
0.00617364200047874,0.0064717827093511),.UNSPECIFIED.);
#1414=B_SPLINE_CURVE_WITH_KNOTS('',3,(#8541,#8542,#8543,#8544,#8545,#8546,
#8547,#8548,#8549,#8550,#8551,#8552,#8553,#8554,#8555,#8556,#8557,#8558,
#8559,#8560,#8561,#8562,#8563,#8564,#8565,#8566,#8567,#8568,#8569,#8570,
#8571,#8572,#8573,#8574,#8575,#8576,#8577,#8578,#8579,#8580,#8581,#8582,
#8583,#8584,#8585,#8586,#8587,#8588,#8589),.UNSPECIFIED.,.F.,.F.,(4,3,3,
3,3,3,3,3,3,3,3,3,3,3,3,3,4),(0.0064898095819301,0.00649606092685136,0.00698916367409277,
0.00748291484157417,0.00797566710589656,0.0081200761585642,0.00857341799443063,
0.00902647257612117,0.00947992094581784,0.00974409139027704,0.0102520995680632,
0.0107611012391323,0.0112695579712555,0.0113681066219899,0.0119417158433385,
0.012514860767218,0.0129921218537027),.UNSPECIFIED.);
#1415=B_SPLINE_CURVE_WITH_KNOTS('',3,(#8590,#8591,#8592,#8593,#8594,#8595,
#8596,#8597,#8598,#8599,#8600,#8601,#8602,#8603,#8604,#8605,#8606,#8607,
#8608,#8609,#8610,#8611,#8612,#8613,#8614,#8615,#8616,#8617,#8618,#8619,
#8620,#8621,#8622,#8623,#8624,#8625,#8626,#8627,#8628,#8629,#8630,#8631,
#8632,#8633,#8634,#8635),.UNSPECIFIED.,.F.,.F.,(4,3,3,3,3,3,3,3,3,3,3,3,
3,3,3,4),(0.,0.000604609839358999,0.00121565628960328,0.00162401523171284,
0.00216471951290587,0.00243602284756926,0.00310314498849404,0.00324803046342568,
0.00365403427135389,0.0040600380792821,0.00451926183054206,0.00487204569513852,
0.00535427083414837,0.00583643300319355,0.0063191303600972,0.0064898095819301),
 .UNSPECIFIED.);
#1416=B_SPLINE_CURVE_WITH_KNOTS('',3,(#8636,#8637,#8638,#8639,#8640,#8641,
#8642,#8643,#8644,#8645,#8646,#8647,#8648,#8649,#8650,#8651,#8652,#8653,
#8654,#8655,#8656,#8657,#8658,#8659,#8660,#8661,#8662,#8663,#8664,#8665,
#8666,#8667,#8668,#8669,#8670,#8671,#8672,#8673,#8674,#8675,#8676,#8677,
#8678,#8679,#8680,#8681),.UNSPECIFIED.,.F.,.F.,(4,3,3,3,3,3,3,3,3,3,3,3,
3,3,3,4),(0.0064717827093511,0.00647607689467181,0.0068808317005888,0.00728558650650579,
0.00779796951019886,0.00809509611833977,0.00863663393440084,0.00917632462956808,
0.00971411534200772,0.0101188701479247,0.0105236249538417,0.0110729177361821,
0.0113331345656757,0.0119056167126292,0.0124755694459539,0.0129521530063804),
 .UNSPECIFIED.);
#1417=B_SPLINE_CURVE_WITH_KNOTS('',3,(#8682,#8683,#8684,#8685,#8686,#8687,
#8688,#8689,#8690,#8691,#8692,#8693,#8694,#8695,#8696,#8697,#8698,#8699,
#8700,#8701,#8702,#8703,#8704,#8705,#8706,#8707,#8708,#8709,#8710,#8711,
#8712,#8713,#8714,#8715,#8716,#8717,#8718,#8719,#8720,#8721,#8722,#8723,
#8724,#8725,#8726,#8727,#8728,#8729,#8730,#8731,#8732,#8733),
 .UNSPECIFIED.,.F.,.F.,(4,3,3,3,3,3,3,3,3,3,3,3,3,3,3,3,3,4),(0.,0.000490776775537461,
0.00073393694656371,0.00124207968922223,0.00155724861738079,0.00162342486873585,
0.00247225450565376,0.00320323287865645,0.00324684973747169,0.00392447218817879,
0.00402584241665628,0.00405856217183962,0.00480782344391585,0.00484857865525814,
0.00487027460620754,0.00567112301456725,0.00568198704057546,0.00648198680776405),
 .UNSPECIFIED.);
#1418=B_SPLINE_CURVE_WITH_KNOTS('',3,(#8735,#8736,#8737,#8738,#8739,#8740,
#8741,#8742,#8743,#8744,#8745),.UNSPECIFIED.,.F.,.F.,(4,1,1,1,1,1,1,1,4),
(0.00648320241242164,0.00649575519632353,0.00730772459586397,0.00811969399540441,
0.00893166339494485,0.00974363279448529,0.0105556021940257,0.0113675715935662,
0.0129915103926471),.UNSPECIFIED.);
#1419=B_SPLINE_CURVE_WITH_KNOTS('',3,(#8748,#8749,#8750,#8751,#8752,#8753,
#8754,#8755,#8756,#8757,#8758,#8759,#8760,#8761,#8762,#8763,#8764,#8765,
#8766,#8767,#8768,#8769,#8770,#8771,#8772,#8773,#8774,#8775,#8776,#8777,
#8778,#8779,#8780,#8781,#8782,#8783,#8784,#8785,#8786,#8787,#8788,#8789,
#8790,#8791,#8792,#8793,#8794,#8795,#8796,#8797,#8798,#8799,#8800,#8801,
#8802),.UNSPECIFIED.,.F.,.F.,(4,3,3,3,3,3,3,3,3,3,3,3,3,3,3,3,3,3,4),(9.20377798281372E-10,
0.000670048056992883,0.000728118409870351,0.000809204961183555,0.00135514668727475,
0.00154786083600147,0.00161840992236711,0.00219729439487813,0.00236979743471876,
0.00242761488355066,0.0031915074931542,0.00323681984473421,0.00401314180766438,
0.00404602480591777,0.00483449084074671,0.00485522976710132,0.00565589261146122,
0.00566443472828487,0.00647004505939142),.UNSPECIFIED.);
#1420=B_SPLINE_CURVE_WITH_KNOTS('',3,(#8803,#8804,#8805,#8806,#8807,#8808,
#8809,#8810,#8811,#8812),.UNSPECIFIED.,.F.,.F.,(4,1,1,1,1,1,1,4),(0.00646652117894175,
0.00646898738861854,0.00727761081219586,0.00808623423577318,0.00970348108292781,
0.0105121045065051,0.0113207279300824,0.0129379736427185),.UNSPECIFIED.);
#1421=B_SPLINE_CURVE_WITH_KNOTS('',3,(#8813,#8814,#8815,#8816,#8817,#8818,
#8819,#8820,#8821,#8822,#8823,#8824,#8825,#8826,#8827,#8828,#8829,#8830,
#8831,#8832,#8833,#8834,#8835,#8836,#8837,#8838,#8839,#8840,#8841,#8842,
#8843,#8844,#8845,#8846,#8847,#8848,#8849,#8850,#8851,#8852,#8853,#8854,
#8855,#8856,#8857,#8858),.UNSPECIFIED.,.F.,.F.,(4,3,3,3,3,3,3,3,3,3,3,3,
3,3,3,4),(0.,0.0004185116728278,0.000735801334826299,0.000812433561769917,
0.00155917246295599,0.00162486712353983,0.00238263123545803,0.00320564025005124,
0.00324973424707967,0.00402847232243131,0.00406216780884958,0.00485131517672913,
0.0048746013706195,0.00567403038972561,0.00568703493238942,0.00648543634797121),
 .UNSPECIFIED.);
#1422=B_SPLINE_CURVE_WITH_KNOTS('',3,(#8859,#8860,#8861,#8862,#8863,#8864,
#8865,#8866,#8867,#8868),.UNSPECIFIED.,.F.,.F.,(4,1,1,1,1,1,1,4),(0.00645802980103412,
0.00645862169996881,0.00726594941246491,0.00807327712496101,0.00968793254995321,
0.0104952602624493,0.0113025879749454,0.0129172416014509),.UNSPECIFIED.);
#1423=B_SPLINE_CURVE_WITH_KNOTS('',3,(#8871,#8872,#8873,#8874,#8875,#8876,
#8877,#8878,#8879,#8880,#8881,#8882),.UNSPECIFIED.,.F.,.F.,(4,2,2,2,2,4),
(-0.362871564393025,-0.274154813883086,-0.182714570720302,-0.100676259181141,
-0.0480732761959632,-4.4821511446802E-8),.UNSPECIFIED.);
#1424=B_SPLINE_CURVE_WITH_KNOTS('',3,(#8883,#8884,#8885,#8886,#8887,#8888,
#8889,#8890,#8891,#8892,#8893,#8894),.UNSPECIFIED.,.F.,.F.,(4,2,2,2,2,4),
(-0.365095457281969,-0.316915096094452,-0.264209783934842,-0.181784066815884,
-0.0898944546920999,-9.99999993344656E-7),.UNSPECIFIED.);
#1425=B_SPLINE_CURVE_WITH_KNOTS('',3,(#8897,#8898,#8899,#8900,#8901,#8902,
#8903,#8904,#8905,#8906,#8907,#8908),.UNSPECIFIED.,.F.,.F.,(4,2,2,2,2,4),
(-0.362873161532576,-0.274151352800392,-0.182714900485669,-0.100677632331331,
-0.0480739883883429,-3.14822323210784E-8),.UNSPECIFIED.);
#1426=B_SPLINE_CURVE_WITH_KNOTS('',3,(#8909,#8910,#8911,#8912,#8913,#8914,
#8915,#8916,#8917,#8918,#8919,#8920),.UNSPECIFIED.,.F.,.F.,(4,2,2,2,2,4),
(-0.365090467953361,-0.316909793473234,-0.264204439712853,-0.18178222731987,
-0.0898981188055125,-9.99999993270273E-7),.UNSPECIFIED.);
#1427=CIRCLE('',#4017,88.0000000000002);
#1428=CIRCLE('',#4018,90.0000000000002);
#1429=CIRCLE('',#4019,90.0000000000002);
#1430=CIRCLE('',#4021,38.);
#1431=CIRCLE('',#4023,56.0000000000002);
#1432=CIRCLE('',#4024,56.0000000000002);
#1433=CIRCLE('',#4025,2.);
#1434=CIRCLE('',#4026,58.0000000000002);
#1435=CIRCLE('',#4027,58.0000000000002);
#1436=CIRCLE('',#4029,30.);
#1437=CIRCLE('',#4030,30.);
#1438=CIRCLE('',#4031,6.00000000000001);
#1439=CIRCLE('',#4032,6.00000000000001);
#1440=CIRCLE('',#4033,6.00000000000001);
#1441=CIRCLE('',#4035,36.);
#1442=CIRCLE('',#4036,30.);
#1443=CIRCLE('',#4038,26.);
#1444=CIRCLE('',#4039,26.);
#1445=CIRCLE('',#4041,25.9999999999999);
#1446=CIRCLE('',#4043,23.9999999999999);
#1447=CIRCLE('',#4045,23.9999999999997);
#1448=CIRCLE('',#4047,83.9999999999997);
#1449=CIRCLE('',#4048,8.);
#1450=CIRCLE('',#4049,8.);
#1451=CIRCLE('',#4050,8.);
#1452=CIRCLE('',#4051,8.);
#1453=CIRCLE('',#4053,83.9999999999998);
#1454=CIRCLE('',#4054,83.9999999999998);
#1455=CIRCLE('',#4056,82.9999999999998);
#1456=CIRCLE('',#4057,8.);
#1457=CIRCLE('',#4058,8.);
#1458=CIRCLE('',#4059,8.);
#1459=CIRCLE('',#4060,8.);
#1460=CIRCLE('',#4061,39.9999999999998);
#1461=CIRCLE('',#4063,39.9999999999999);
#1462=CIRCLE('',#4064,39.9999999999999);
#1463=CIRCLE('',#4066,2.);
#1464=CIRCLE('',#4067,42.);
#1465=CIRCLE('',#4069,47.9999999999999);
#1466=CIRCLE('',#4071,8.);
#1467=CIRCLE('',#4072,56.);
#1468=CIRCLE('',#4073,56.);
#1469=CIRCLE('',#4074,56.);
#1470=CIRCLE('',#4077,90.0000000000003);
#1471=CIRCLE('',#4079,40.999999999998);
#1472=CIRCLE('',#4080,6.00000000000001);
#1473=CIRCLE('',#4081,6.00000000000001);
#1474=CIRCLE('',#4082,6.00000000000001);
#1475=CIRCLE('',#4083,6.00000000000001);
#1476=CIRCLE('',#4085,39.999999999998);
#1477=CIRCLE('',#4086,39.999999999998);
#1478=CIRCLE('',#4087,39.999999999998);
#1479=CIRCLE('',#4089,44.0000000000002);
#1480=CIRCLE('',#4091,44.);
#1481=CIRCLE('',#4093,38.5);
#1482=CIRCLE('',#4095,2.5);
#1483=CIRCLE('',#4097,84.);
#1484=CIRCLE('',#4098,84.);
#1485=CIRCLE('',#4100,8.);
#1486=CIRCLE('',#4101,8.);
#1487=CIRCLE('',#4102,8.);
#1488=CIRCLE('',#4103,8.);
#1489=CIRCLE('',#4105,8.);
#1490=CIRCLE('',#4106,8.);
#1491=CIRCLE('',#4107,8.);
#1492=CIRCLE('',#4108,8.);
#1493=CIRCLE('',#4109,24.);
#1494=CIRCLE('',#4123,6.00000000000002);
#1495=CIRCLE('',#4124,6.00000000000002);
#1496=CIRCLE('',#4132,1.);
#1497=CIRCLE('',#4134,1.);
#1498=CIRCLE('',#4137,26.);
#1499=CIRCLE('',#4139,26.);
#1500=CIRCLE('',#4141,26.);
#1501=CIRCLE('',#4143,26.);
#1502=CIRCLE('',#4149,24.);
#1503=CIRCLE('',#4150,11.);
#1504=CIRCLE('',#4152,24.);
#1505=CIRCLE('',#4153,24.);
#1506=CIRCLE('',#4154,24.);
#1507=CIRCLE('',#4155,24.);
#1508=CIRCLE('',#4156,24.);
#1509=CIRCLE('',#4158,30.);
#1510=CIRCLE('',#4160,30.);
#1511=CIRCLE('',#4161,30.);
#1512=CIRCLE('',#4163,26.);
#1513=CIRCLE('',#4164,26.);
#1514=CIRCLE('',#4165,26.);
#1515=CIRCLE('',#4166,26.);
#1516=CIRCLE('',#4167,26.);
#1517=CIRCLE('',#4170,11.);
#1518=CIRCLE('',#4174,26.);
#1519=CIRCLE('',#4176,26.);
#1520=CIRCLE('',#4178,22.);
#1521=CIRCLE('',#4179,22.);
#1522=CIRCLE('',#4180,22.);
#1523=CIRCLE('',#4181,22.);
#1524=CIRCLE('',#4185,26.);
#1525=CIRCLE('',#4189,26.);
#1526=CIRCLE('',#4196,6.);
#1527=CIRCLE('',#4198,6.);
#1528=CIRCLE('',#4200,6.);
#1529=CIRCLE('',#4202,7.);
#1530=CIRCLE('',#4204,9.99999999999995);
#1531=CIRCLE('',#4206,10.);
#1532=CIRCLE('',#4208,7.99999999999999);
#1533=CIRCLE('',#4210,8.);
#1534=CIRCLE('',#4213,1.);
#1535=CIRCLE('',#4219,6.);
#1536=CIRCLE('',#4221,6.);
#1537=CIRCLE('',#4225,14.);
#1538=CIRCLE('',#4226,8.);
#1539=CIRCLE('',#4228,14.);
#1540=CIRCLE('',#4229,8.);
#1541=CIRCLE('',#4236,2.);
#1542=CIRCLE('',#4237,1.5);
#1543=CIRCLE('',#4242,25.999999999998);
#1544=CIRCLE('',#4243,18.0000000000002);
#1545=CIRCLE('',#4245,18.);
#1546=CIRCLE('',#4246,18.);
#1547=CIRCLE('',#4248,10.);
#1548=CIRCLE('',#4249,10.);
#1549=CIRCLE('',#4251,9.9999999999999);
#1550=CIRCLE('',#4253,19.9999999999999);
#1551=CIRCLE('',#4255,28.);
#1552=CIRCLE('',#4257,40.);
#1553=CIRCLE('',#4259,40.);
#1554=CIRCLE('',#4261,89.999999999998);
#1555=CIRCLE('',#4262,6.);
#1556=CIRCLE('',#4263,6.);
#1557=CIRCLE('',#4264,6.);
#1558=CIRCLE('',#4265,6.);
#1559=CIRCLE('',#4267,89.999999999998);
#1560=CIRCLE('',#4269,6.);
#1561=CIRCLE('',#4270,6.);
#1562=CIRCLE('',#4271,6.);
#1563=CIRCLE('',#4272,6.);
#1564=CIRCLE('',#4273,25.9999999999979);
#1565=CIRCLE('',#4281,10.0000000000001);
#1566=CIRCLE('',#4282,10.);
#1567=CIRCLE('',#4284,22.0000000000001);
#1568=CIRCLE('',#4286,22.);
#1569=CIRCLE('',#4288,18.);
#1570=CIRCLE('',#4290,18.);
#1571=CIRCLE('',#4300,26.);
#1572=CIRCLE('',#4302,26.);
#1573=CIRCLE('',#4304,12.);
#1574=CIRCLE('',#4306,34.6410161513776);
#1575=CIRCLE('',#4308,34.6410161513776);
#1576=CIRCLE('',#4310,34.6410161513776);
#1577=CIRCLE('',#4312,34.6410161513776);
#1578=CIRCLE('',#4314,34.6410161513776);
#1579=CIRCLE('',#4316,34.6410161513776);
#1580=CIRCLE('',#4318,20.);
#1581=CIRCLE('',#4319,10.);
#1582=CIRCLE('',#4322,12.);
#1583=CIRCLE('',#4324,10.);
#1584=CIRCLE('',#4330,18.);
#1585=CIRCLE('',#4331,71.);
#1586=CIRCLE('',#4333,18.);
#1587=CIRCLE('',#4334,71.);
#1588=CIRCLE('',#4335,71.);
#1589=CIRCLE('',#4337,18.);
#1590=CIRCLE('',#4338,71.);
#1591=CIRCLE('',#4340,18.);
#1592=CIRCLE('',#4341,71.);
#1593=CIRCLE('',#4342,71.);
#1594=CIRCLE('',#4344,18.);
#1595=CIRCLE('',#4345,71.);
#1596=CIRCLE('',#4347,18.);
#1597=CIRCLE('',#4348,71.);
#1598=CIRCLE('',#4356,10.);
#1599=CIRCLE('',#4357,69.);
#1600=CIRCLE('',#4358,71.);
#1601=CIRCLE('',#4359,69.);
#1602=CIRCLE('',#4360,69.);
#1603=CIRCLE('',#4361,69.);
#1604=CIRCLE('',#4362,71.);
#1605=CIRCLE('',#4364,18.);
#1606=CIRCLE('',#4366,18.);
#1607=CIRCLE('',#4368,16.);
#1608=CIRCLE('',#4369,16.);
#1609=CIRCLE('',#4370,16.);
#1610=CIRCLE('',#4371,16.);
#1611=CIRCLE('',#4372,16.);
#1612=CIRCLE('',#4373,16.);
#1613=CIRCLE('',#4374,16.);
#1614=CIRCLE('',#4375,16.);
#1615=CIRCLE('',#4376,16.);
#1616=CIRCLE('',#4377,16.);
#1617=CIRCLE('',#4378,16.);
#1618=CIRCLE('',#4379,16.);
#1619=CIRCLE('',#4402,10.3923048454133);
#1620=CIRCLE('',#4403,10.3923048454133);
#1621=CIRCLE('',#4404,10.3923048454133);
#1622=CIRCLE('',#4405,10.3923048454133);
#1623=CIRCLE('',#4406,10.3923048454133);
#1624=CIRCLE('',#4407,10.3923048454133);
#1625=CIRCLE('',#4408,6.);
#1626=CIRCLE('',#4410,10.3923048454133);
#1627=CIRCLE('',#4411,10.3923048454133);
#1628=CIRCLE('',#4412,10.3923048454133);
#1629=CIRCLE('',#4413,10.3923048454133);
#1630=CIRCLE('',#4414,10.3923048454133);
#1631=CIRCLE('',#4415,10.3923048454133);
#1632=CIRCLE('',#4416,6.);
#1633=CIRCLE('',#4438,6.);
#1634=CIRCLE('',#4439,6.);
#1635=CIRCLE('',#4443,10.3923048454133);
#1636=CIRCLE('',#4445,10.3923048454133);
#1637=CIRCLE('',#4447,10.3923048454133);
#1638=CIRCLE('',#4449,10.3923048454133);
#1639=CIRCLE('',#4451,10.3923048454133);
#1640=CIRCLE('',#4453,10.3923048454133);
#1641=VERTEX_POINT('',#5573);
#1642=VERTEX_POINT('',#5574);
#1643=VERTEX_POINT('',#5576);
#1644=VERTEX_POINT('',#5585);
#1645=VERTEX_POINT('',#5587);
#1646=VERTEX_POINT('',#5600);
#1647=VERTEX_POINT('',#5601);
#1648=VERTEX_POINT('',#5636);
#1649=VERTEX_POINT('',#5638);
#1650=VERTEX_POINT('',#5657);
#1651=VERTEX_POINT('',#5668);
#1652=VERTEX_POINT('',#5687);
#1653=VERTEX_POINT('',#5691);
#1654=VERTEX_POINT('',#5706);
#1655=VERTEX_POINT('',#5776);
#1656=VERTEX_POINT('',#5777);
#1657=VERTEX_POINT('',#5780);
#1658=VERTEX_POINT('',#5782);
#1659=VERTEX_POINT('',#5784);
#1660=VERTEX_POINT('',#5795);
#1661=VERTEX_POINT('',#5980);
#1662=VERTEX_POINT('',#5993);
#1663=VERTEX_POINT('',#5996);
#1664=VERTEX_POINT('',#5999);
#1665=VERTEX_POINT('',#6001);
#1666=VERTEX_POINT('',#6003);
#1667=VERTEX_POINT('',#6006);
#1668=VERTEX_POINT('',#6008);
#1669=VERTEX_POINT('',#6011);
#1670=VERTEX_POINT('',#6012);
#1671=VERTEX_POINT('',#6017);
#1672=VERTEX_POINT('',#6021);
#1673=VERTEX_POINT('',#6024);
#1674=VERTEX_POINT('',#6028);
#1675=VERTEX_POINT('',#6030);
#1676=VERTEX_POINT('',#6032);
#1677=VERTEX_POINT('',#6034);
#1678=VERTEX_POINT('',#6036);
#1679=VERTEX_POINT('',#6039);
#1680=VERTEX_POINT('',#6041);
#1681=VERTEX_POINT('',#6045);
#1682=VERTEX_POINT('',#6047);
#1683=VERTEX_POINT('',#6049);
#1684=VERTEX_POINT('',#6051);
#1685=VERTEX_POINT('',#6053);
#1686=VERTEX_POINT('',#6055);
#1687=VERTEX_POINT('',#6058);
#1688=VERTEX_POINT('',#6060);
#1689=VERTEX_POINT('',#6064);
#1690=VERTEX_POINT('',#6068);
#1691=VERTEX_POINT('',#6071);
#1692=VERTEX_POINT('',#6073);
#1693=VERTEX_POINT('',#6081);
#1694=VERTEX_POINT('',#6086);
#1695=VERTEX_POINT('',#6088);
#1696=VERTEX_POINT('',#6090);
#1697=VERTEX_POINT('',#6092);
#1698=VERTEX_POINT('',#6094);
#1699=VERTEX_POINT('',#6097);
#1700=VERTEX_POINT('',#6098);
#1701=VERTEX_POINT('',#6101);
#1702=VERTEX_POINT('',#6105);
#1703=VERTEX_POINT('',#6108);
#1704=VERTEX_POINT('',#6111);
#1705=VERTEX_POINT('',#6112);
#1706=VERTEX_POINT('',#6182);
#1707=VERTEX_POINT('',#6187);
#1708=VERTEX_POINT('',#6189);
#1709=VERTEX_POINT('',#6193);
#1710=VERTEX_POINT('',#6195);
#1711=VERTEX_POINT('',#6197);
#1712=VERTEX_POINT('',#6199);
#1713=VERTEX_POINT('',#6202);
#1714=VERTEX_POINT('',#6204);
#1715=VERTEX_POINT('',#6206);
#1716=VERTEX_POINT('',#6208);
#1717=VERTEX_POINT('',#6210);
#1718=VERTEX_POINT('',#6238);
#1719=VERTEX_POINT('',#6240);
#1720=VERTEX_POINT('',#6244);
#1721=VERTEX_POINT('',#6260);
#1722=VERTEX_POINT('',#6261);
#1723=VERTEX_POINT('',#6263);
#1724=VERTEX_POINT('',#6267);
#1725=VERTEX_POINT('',#6268);
#1726=VERTEX_POINT('',#6270);
#1727=VERTEX_POINT('',#6274);
#1728=VERTEX_POINT('',#6275);
#1729=VERTEX_POINT('',#6277);
#1730=VERTEX_POINT('',#6281);
#1731=VERTEX_POINT('',#6282);
#1732=VERTEX_POINT('',#6284);
#1733=VERTEX_POINT('',#6288);
#1734=VERTEX_POINT('',#6290);
#1735=VERTEX_POINT('',#6294);
#1736=VERTEX_POINT('',#6298);
#1737=VERTEX_POINT('',#6299);
#1738=VERTEX_POINT('',#6301);
#1739=VERTEX_POINT('',#6308);
#1740=VERTEX_POINT('',#6309);
#1741=VERTEX_POINT('',#6311);
#1742=VERTEX_POINT('',#6318);
#1743=VERTEX_POINT('',#6320);
#1744=VERTEX_POINT('',#6324);
#1745=VERTEX_POINT('',#6328);
#1746=VERTEX_POINT('',#6330);
#1747=VERTEX_POINT('',#6333);
#1748=VERTEX_POINT('',#6334);
#1749=VERTEX_POINT('',#6336);
#1750=VERTEX_POINT('',#6339);
#1751=VERTEX_POINT('',#6341);
#1752=VERTEX_POINT('',#6343);
#1753=VERTEX_POINT('',#6345);
#1754=VERTEX_POINT('',#6347);
#1755=VERTEX_POINT('',#6349);
#1756=VERTEX_POINT('',#6353);
#1757=VERTEX_POINT('',#6358);
#1758=VERTEX_POINT('',#6359);
#1759=VERTEX_POINT('',#6364);
#1760=VERTEX_POINT('',#6375);
#1761=VERTEX_POINT('',#6385);
#1762=VERTEX_POINT('',#6387);
#1763=VERTEX_POINT('',#6391);
#1764=VERTEX_POINT('',#6393);
#1765=VERTEX_POINT('',#6398);
#1766=VERTEX_POINT('',#6404);
#1767=VERTEX_POINT('',#6412);
#1768=VERTEX_POINT('',#6418);
#1769=VERTEX_POINT('',#6431);
#1770=VERTEX_POINT('',#6432);
#1771=VERTEX_POINT('',#6434);
#1772=VERTEX_POINT('',#6438);
#1773=VERTEX_POINT('',#6440);
#1774=VERTEX_POINT('',#6444);
#1775=VERTEX_POINT('',#6446);
#1776=VERTEX_POINT('',#6450);
#1777=VERTEX_POINT('',#6453);
#1778=VERTEX_POINT('',#6455);
#1779=VERTEX_POINT('',#6456);
#1780=VERTEX_POINT('',#6458);
#1781=VERTEX_POINT('',#6460);
#1782=VERTEX_POINT('',#6464);
#1783=VERTEX_POINT('',#6468);
#1784=VERTEX_POINT('',#6471);
#1785=VERTEX_POINT('',#6474);
#1786=VERTEX_POINT('',#6475);
#1787=VERTEX_POINT('',#6512);
#1788=VERTEX_POINT('',#6513);
#1789=VERTEX_POINT('',#6556);
#1790=VERTEX_POINT('',#6568);
#1791=VERTEX_POINT('',#6574);
#1792=VERTEX_POINT('',#6576);
#1793=VERTEX_POINT('',#6579);
#1794=VERTEX_POINT('',#6581);
#1795=VERTEX_POINT('',#6584);
#1796=VERTEX_POINT('',#6586);
#1797=VERTEX_POINT('',#6595);
#1798=VERTEX_POINT('',#6602);
#1799=VERTEX_POINT('',#6632);
#1800=VERTEX_POINT('',#6633);
#1801=VERTEX_POINT('',#6673);
#1802=VERTEX_POINT('',#6675);
#1803=VERTEX_POINT('',#6686);
#1804=VERTEX_POINT('',#6693);
#1805=VERTEX_POINT('',#6721);
#1806=VERTEX_POINT('',#6722);
#1807=VERTEX_POINT('',#6767);
#1808=VERTEX_POINT('',#6769);
#1809=VERTEX_POINT('',#6776);
#1810=VERTEX_POINT('',#6778);
#1811=VERTEX_POINT('',#6781);
#1812=VERTEX_POINT('',#6783);
#1813=VERTEX_POINT('',#6787);
#1814=VERTEX_POINT('',#6788);
#1815=VERTEX_POINT('',#6793);
#1816=VERTEX_POINT('',#6797);
#1817=VERTEX_POINT('',#6800);
#1818=VERTEX_POINT('',#6804);
#1819=VERTEX_POINT('',#6807);
#1820=VERTEX_POINT('',#6811);
#1821=VERTEX_POINT('',#6813);
#1822=VERTEX_POINT('',#6815);
#1823=VERTEX_POINT('',#6817);
#1824=VERTEX_POINT('',#6819);
#1825=VERTEX_POINT('',#6822);
#1826=VERTEX_POINT('',#6826);
#1827=VERTEX_POINT('',#6828);
#1828=VERTEX_POINT('',#6830);
#1829=VERTEX_POINT('',#6832);
#1830=VERTEX_POINT('',#6834);
#1831=VERTEX_POINT('',#6848);
#1832=VERTEX_POINT('',#6850);
#1833=VERTEX_POINT('',#6854);
#1834=VERTEX_POINT('',#6857);
#1835=VERTEX_POINT('',#6861);
#1836=VERTEX_POINT('',#6864);
#1837=VERTEX_POINT('',#6871);
#1838=VERTEX_POINT('',#6872);
#1839=VERTEX_POINT('',#6874);
#1840=VERTEX_POINT('',#6897);
#1841=VERTEX_POINT('',#6920);
#1842=VERTEX_POINT('',#6924);
#1843=VERTEX_POINT('',#6925);
#1844=VERTEX_POINT('',#6927);
#1845=VERTEX_POINT('',#6966);
#1846=VERTEX_POINT('',#6967);
#1847=VERTEX_POINT('',#7004);
#1848=VERTEX_POINT('',#7008);
#1849=VERTEX_POINT('',#7009);
#1850=VERTEX_POINT('',#7011);
#1851=VERTEX_POINT('',#7050);
#1852=VERTEX_POINT('',#7051);
#1853=VERTEX_POINT('',#7053);
#1854=VERTEX_POINT('',#7092);
#1855=VERTEX_POINT('',#7131);
#1856=VERTEX_POINT('',#7134);
#1857=VERTEX_POINT('',#7138);
#1858=VERTEX_POINT('',#7153);
#1859=VERTEX_POINT('',#7155);
#1860=VERTEX_POINT('',#7160);
#1861=VERTEX_POINT('',#7164);
#1862=VERTEX_POINT('',#7170);
#1863=VERTEX_POINT('',#7171);
#1864=VERTEX_POINT('',#7173);
#1865=VERTEX_POINT('',#7262);
#1866=VERTEX_POINT('',#7264);
#1867=VERTEX_POINT('',#7275);
#1868=VERTEX_POINT('',#7288);
#1869=VERTEX_POINT('',#7289);
#1870=VERTEX_POINT('',#7291);
#1871=VERTEX_POINT('',#7383);
#1872=VERTEX_POINT('',#7385);
#1873=VERTEX_POINT('',#7396);
#1874=VERTEX_POINT('',#7410);
#1875=VERTEX_POINT('',#7423);
#1876=VERTEX_POINT('',#7438);
#1877=VERTEX_POINT('',#7439);
#1878=VERTEX_POINT('',#7441);
#1879=VERTEX_POINT('',#7443);
#1880=VERTEX_POINT('',#7445);
#1881=VERTEX_POINT('',#7458);
#1882=VERTEX_POINT('',#7460);
#1883=VERTEX_POINT('',#7475);
#1884=VERTEX_POINT('',#7476);
#1885=VERTEX_POINT('',#7478);
#1886=VERTEX_POINT('',#7480);
#1887=VERTEX_POINT('',#7482);
#1888=VERTEX_POINT('',#7495);
#1889=VERTEX_POINT('',#7510);
#1890=VERTEX_POINT('',#7511);
#1891=VERTEX_POINT('',#7513);
#1892=VERTEX_POINT('',#7515);
#1893=VERTEX_POINT('',#7517);
#1894=VERTEX_POINT('',#7530);
#1895=VERTEX_POINT('',#7532);
#1896=VERTEX_POINT('',#7548);
#1897=VERTEX_POINT('',#7561);
#1898=VERTEX_POINT('',#7576);
#1899=VERTEX_POINT('',#7577);
#1900=VERTEX_POINT('',#7579);
#1901=VERTEX_POINT('',#7581);
#1902=VERTEX_POINT('',#7583);
#1903=VERTEX_POINT('',#7596);
#1904=VERTEX_POINT('',#7611);
#1905=VERTEX_POINT('',#7700);
#1906=VERTEX_POINT('',#7702);
#1907=VERTEX_POINT('',#7713);
#1908=VERTEX_POINT('',#7726);
#1909=VERTEX_POINT('',#7727);
#1910=VERTEX_POINT('',#7811);
#1911=VERTEX_POINT('',#7822);
#1912=VERTEX_POINT('',#7920);
#1913=VERTEX_POINT('',#7931);
#1914=VERTEX_POINT('',#8032);
#1915=VERTEX_POINT('',#8043);
#1916=VERTEX_POINT('',#8056);
#1917=VERTEX_POINT('',#8148);
#1918=VERTEX_POINT('',#8150);
#1919=VERTEX_POINT('',#8161);
#1920=VERTEX_POINT('',#8174);
#1921=VERTEX_POINT('',#8175);
#1922=VERTEX_POINT('',#8262);
#1923=VERTEX_POINT('',#8273);
#1924=VERTEX_POINT('',#8287);
#1925=VERTEX_POINT('',#8298);
#1926=VERTEX_POINT('',#8300);
#1927=VERTEX_POINT('',#8353);
#1928=VERTEX_POINT('',#8355);
#1929=VERTEX_POINT('',#8367);
#1930=VERTEX_POINT('',#8424);
#1931=VERTEX_POINT('',#8435);
#1932=VERTEX_POINT('',#8495);
#1933=VERTEX_POINT('',#8539);
#1934=VERTEX_POINT('',#8734);
#1935=VERTEX_POINT('',#8746);
#1936=VERTEX_POINT('',#8922);
#1937=VERTEX_POINT('',#8924);
#1938=VERTEX_POINT('',#8927);
#1939=VERTEX_POINT('',#8929);
#1940=VERTEX_POINT('',#8941);
#1941=VERTEX_POINT('',#8942);
#1942=VERTEX_POINT('',#8944);
#1943=VERTEX_POINT('',#8946);
#1944=VERTEX_POINT('',#8950);
#1945=VERTEX_POINT('',#8951);
#1946=VERTEX_POINT('',#8953);
#1947=VERTEX_POINT('',#8955);
#1948=VERTEX_POINT('',#9396);
#1949=VERTEX_POINT('',#9397);
#1950=VERTEX_POINT('',#9401);
#1951=VERTEX_POINT('',#9403);
#1952=VERTEX_POINT('',#9407);
#1953=VERTEX_POINT('',#9411);
#1954=VERTEX_POINT('',#9417);
#1955=VERTEX_POINT('',#9418);
#1956=VERTEX_POINT('',#9422);
#1957=VERTEX_POINT('',#9424);
#1958=VERTEX_POINT('',#9435);
#1959=VERTEX_POINT('',#9436);
#1960=VERTEX_POINT('',#9440);
#1961=VERTEX_POINT('',#9442);
#1962=VERTEX_POINT('',#9453);
#1963=VERTEX_POINT('',#9454);
#1964=VERTEX_POINT('',#9458);
#1965=VERTEX_POINT('',#9460);
#1966=VERTEX_POINT('',#9471);
#1967=VERTEX_POINT('',#9472);
#1968=VERTEX_POINT('',#9476);
#1969=VERTEX_POINT('',#9478);
#1970=VERTEX_POINT('',#9489);
#1971=VERTEX_POINT('',#9493);
#1972=VERTEX_POINT('',#9510);
#1973=VERTEX_POINT('',#9519);
#1974=VERTEX_POINT('',#9537);
#1975=VERTEX_POINT('',#9538);
#1976=VERTEX_POINT('',#9542);
#1977=VERTEX_POINT('',#9544);
#1978=VERTEX_POINT('',#9546);
#1979=VERTEX_POINT('',#9552);
#1980=VERTEX_POINT('',#9556);
#1981=VERTEX_POINT('',#9558);
#1982=VERTEX_POINT('',#9564);
#1983=VERTEX_POINT('',#9568);
#1984=VERTEX_POINT('',#9570);
#1985=VERTEX_POINT('',#9576);
#1986=VERTEX_POINT('',#9580);
#1987=VERTEX_POINT('',#9582);
#1988=VERTEX_POINT('',#9588);
#1989=VERTEX_POINT('',#9592);
#1990=VERTEX_POINT('',#9594);
#1991=VERTEX_POINT('',#9600);
#1992=VERTEX_POINT('',#9609);
#1993=VERTEX_POINT('',#9611);
#1994=EDGE_CURVE('',#1641,#1642,#1427,.T.);
#1995=EDGE_CURVE('',#1641,#1643,#1329,.T.);
#1996=EDGE_CURVE('',#1643,#1644,#1428,.T.);
#1997=EDGE_CURVE('',#1644,#1645,#1429,.T.);
#1998=EDGE_CURVE('',#1645,#1642,#1330,.F.);
#1999=EDGE_CURVE('',#1646,#1647,#1331,.T.);
#2000=EDGE_CURVE('',#1647,#1648,#371,.T.);
#2001=EDGE_CURVE('',#1648,#1649,#1332,.F.);
#2002=EDGE_CURVE('',#1649,#1650,#1333,.T.);
#2003=EDGE_CURVE('',#1650,#1651,#1334,.T.);
#2004=EDGE_CURVE('',#1652,#1651,#372,.T.);
#2005=EDGE_CURVE('',#1652,#1652,#1430,.F.);
#2006=EDGE_CURVE('',#1651,#1646,#373,.T.);
#2007=EDGE_CURVE('',#1646,#1653,#1335,.T.);
#2008=EDGE_CURVE('',#1653,#1654,#1336,.T.);
#2009=EDGE_CURVE('',#1654,#1646,#1337,.T.);
#2010=EDGE_CURVE('',#1655,#1656,#1431,.T.);
#2011=EDGE_CURVE('',#1656,#1655,#1432,.T.);
#2012=EDGE_CURVE('',#1656,#1657,#1433,.T.);
#2013=EDGE_CURVE('',#1657,#1658,#1434,.T.);
#2014=EDGE_CURVE('',#1658,#1659,#1338,.T.);
#2015=EDGE_CURVE('',#1659,#1660,#1339,.T.);
#2016=EDGE_CURVE('',#1660,#1661,#1340,.T.);
#2017=EDGE_CURVE('',#1661,#1657,#1435,.T.);
#2018=EDGE_CURVE('',#1642,#1662,#1436,.F.);
#2019=EDGE_CURVE('',#1658,#1662,#374,.T.);
#2020=EDGE_CURVE('',#1663,#1661,#375,.T.);
#2021=EDGE_CURVE('',#1663,#1641,#1437,.F.);
#2022=EDGE_CURVE('',#1664,#1664,#1438,.T.);
#2023=EDGE_CURVE('',#1665,#1665,#1439,.T.);
#2024=EDGE_CURVE('',#1666,#1666,#1440,.T.);
#2025=EDGE_CURVE('',#1667,#1667,#1441,.T.);
#2026=EDGE_CURVE('',#1668,#1668,#1442,.T.);
#2027=EDGE_CURVE('',#1669,#1670,#1443,.T.);
#2028=EDGE_CURVE('',#1670,#1669,#1444,.T.);
#2029=EDGE_CURVE('',#1669,#1668,#376,.T.);
#2030=EDGE_CURVE('',#1670,#1671,#377,.T.);
#2031=EDGE_CURVE('',#1671,#1671,#1445,.T.);
#2032=EDGE_CURVE('',#1672,#1672,#1446,.T.);
#2033=EDGE_CURVE('',#1672,#1673,#378,.T.);
#2034=EDGE_CURVE('',#1673,#1673,#1447,.T.);
#2035=EDGE_CURVE('',#1674,#1674,#1448,.T.);
#2036=EDGE_CURVE('',#1675,#1675,#1449,.T.);
#2037=EDGE_CURVE('',#1676,#1676,#1450,.T.);
#2038=EDGE_CURVE('',#1677,#1677,#1451,.T.);
#2039=EDGE_CURVE('',#1678,#1678,#1452,.T.);
#2040=EDGE_CURVE('',#1674,#1679,#379,.T.);
#2041=EDGE_CURVE('',#1679,#1680,#1453,.F.);
#2042=EDGE_CURVE('',#1680,#1679,#1454,.F.);
#2043=EDGE_CURVE('',#1681,#1681,#1455,.T.);
#2044=EDGE_CURVE('',#1682,#1682,#1456,.F.);
#2045=EDGE_CURVE('',#1683,#1683,#1457,.F.);
#2046=EDGE_CURVE('',#1684,#1684,#1458,.F.);
#2047=EDGE_CURVE('',#1685,#1685,#1459,.F.);
#2048=EDGE_CURVE('',#1686,#1686,#1460,.T.);
#2049=EDGE_CURVE('',#1686,#1687,#380,.T.);
#2050=EDGE_CURVE('',#1687,#1688,#1461,.T.);
#2051=EDGE_CURVE('',#1688,#1687,#1462,.T.);
#2052=EDGE_CURVE('',#1688,#1689,#1463,.T.);
#2053=EDGE_CURVE('',#1689,#1689,#1464,.T.);
#2054=EDGE_CURVE('',#1690,#1690,#1465,.T.);
#2055=EDGE_CURVE('',#1690,#1691,#1466,.T.);
#2056=EDGE_CURVE('',#1691,#1692,#1467,.T.);
#2057=EDGE_CURVE('',#1692,#1654,#1468,.T.);
#2058=EDGE_CURVE('',#1653,#1691,#1469,.T.);
#2059=EDGE_CURVE('',#1692,#1655,#381,.T.);
#2060=EDGE_CURVE('',#1649,#1645,#382,.F.);
#2061=EDGE_CURVE('',#1644,#1693,#383,.T.);
#2062=EDGE_CURVE('',#1693,#1693,#1470,.T.);
#2063=EDGE_CURVE('',#1643,#1650,#384,.T.);
#2064=EDGE_CURVE('',#1694,#1694,#1471,.F.);
#2065=EDGE_CURVE('',#1695,#1695,#1472,.T.);
#2066=EDGE_CURVE('',#1696,#1696,#1473,.T.);
#2067=EDGE_CURVE('',#1697,#1697,#1474,.T.);
#2068=EDGE_CURVE('',#1698,#1698,#1475,.T.);
#2069=EDGE_CURVE('',#1699,#1700,#1476,.T.);
#2070=EDGE_CURVE('',#1700,#1699,#1477,.T.);
#2071=EDGE_CURVE('',#1699,#1701,#385,.T.);
#2072=EDGE_CURVE('',#1701,#1701,#1478,.T.);
#2073=EDGE_CURVE('',#1702,#1702,#1479,.T.);
#2074=EDGE_CURVE('',#1702,#1703,#386,.T.);
#2075=EDGE_CURVE('',#1703,#1703,#1480,.T.);
#2076=EDGE_CURVE('',#1704,#1705,#1341,.T.);
#2077=EDGE_CURVE('',#1705,#1704,#1342,.T.);
#2078=EDGE_CURVE('',#1706,#1706,#1481,.T.);
#2079=EDGE_CURVE('',#1706,#1667,#1482,.T.);
#2080=EDGE_CURVE('',#1707,#1707,#1483,.T.);
#2081=EDGE_CURVE('',#1707,#1708,#387,.T.);
#2082=EDGE_CURVE('',#1708,#1708,#1484,.T.);
#2083=EDGE_CURVE('',#1709,#1709,#1485,.F.);
#2084=EDGE_CURVE('',#1710,#1710,#1486,.F.);
#2085=EDGE_CURVE('',#1711,#1711,#1487,.F.);
#2086=EDGE_CURVE('',#1712,#1712,#1488,.F.);
#2087=EDGE_CURVE('',#1713,#1713,#1489,.T.);
#2088=EDGE_CURVE('',#1714,#1714,#1490,.T.);
#2089=EDGE_CURVE('',#1715,#1715,#1491,.T.);
#2090=EDGE_CURVE('',#1716,#1716,#1492,.T.);
#2091=EDGE_CURVE('',#1717,#1717,#1493,.T.);
#2092=EDGE_CURVE('',#1646,#1660,#388,.T.);
#2093=EDGE_CURVE('',#1647,#1659,#389,.T.);
#2094=EDGE_CURVE('',#1662,#1648,#390,.F.);
#2095=EDGE_CURVE('',#1651,#1663,#391,.T.);
#2096=EDGE_CURVE('',#1705,#1717,#392,.T.);
#2097=EDGE_CURVE('',#1712,#1716,#393,.T.);
#2098=EDGE_CURVE('',#1711,#1715,#394,.T.);
#2099=EDGE_CURVE('',#1710,#1714,#395,.T.);
#2100=EDGE_CURVE('',#1709,#1713,#396,.T.);
#2101=EDGE_CURVE('',#1685,#1678,#397,.T.);
#2102=EDGE_CURVE('',#1684,#1677,#398,.T.);
#2103=EDGE_CURVE('',#1683,#1676,#399,.T.);
#2104=EDGE_CURVE('',#1682,#1675,#400,.T.);
#2105=EDGE_CURVE('',#1698,#1718,#401,.T.);
#2106=EDGE_CURVE('',#1718,#1719,#1494,.T.);
#2107=EDGE_CURVE('',#1719,#1718,#1495,.T.);
#2108=EDGE_CURVE('',#1720,#1719,#402,.T.);
#2109=EDGE_CURVE('',#1697,#1666,#403,.T.);
#2110=EDGE_CURVE('',#1696,#1665,#404,.T.);
#2111=EDGE_CURVE('',#1695,#1664,#405,.T.);
#2112=EDGE_CURVE('',#1700,#1694,#1496,.T.);
#2113=EDGE_CURVE('',#1681,#1680,#1497,.T.);
#2114=EDGE_CURVE('',#1721,#1722,#1498,.T.);
#2115=EDGE_CURVE('',#1723,#1722,#406,.T.);
#2116=EDGE_CURVE('',#1721,#1723,#407,.T.);
#2117=EDGE_CURVE('',#1724,#1725,#408,.T.);
#2118=EDGE_CURVE('',#1726,#1724,#409,.T.);
#2119=EDGE_CURVE('',#1726,#1725,#1499,.T.);
#2120=EDGE_CURVE('',#1727,#1728,#410,.T.);
#2121=EDGE_CURVE('',#1729,#1727,#411,.T.);
#2122=EDGE_CURVE('',#1729,#1728,#1500,.T.);
#2123=EDGE_CURVE('',#1730,#1731,#1501,.T.);
#2124=EDGE_CURVE('',#1732,#1731,#412,.T.);
#2125=EDGE_CURVE('',#1730,#1732,#413,.T.);
#2126=EDGE_CURVE('',#1733,#1728,#414,.T.);
#2127=EDGE_CURVE('',#1733,#1734,#75,.T.);
#2128=EDGE_CURVE('',#1735,#1734,#415,.T.);
#2129=EDGE_CURVE('',#1727,#1735,#416,.T.);
#2130=EDGE_CURVE('',#1736,#1737,#417,.T.);
#2131=EDGE_CURVE('',#1736,#1738,#76,.T.);
#2132=EDGE_CURVE('',#1738,#1730,#418,.T.);
#2133=EDGE_CURVE('',#1737,#1732,#419,.T.);
#2134=EDGE_CURVE('',#1739,#1740,#420,.T.);
#2135=EDGE_CURVE('',#1739,#1741,#77,.T.);
#2136=EDGE_CURVE('',#1741,#1721,#421,.T.);
#2137=EDGE_CURVE('',#1740,#1723,#422,.T.);
#2138=EDGE_CURVE('',#1742,#1725,#423,.T.);
#2139=EDGE_CURVE('',#1742,#1743,#78,.T.);
#2140=EDGE_CURVE('',#1744,#1743,#424,.T.);
#2141=EDGE_CURVE('',#1724,#1744,#425,.T.);
#2142=EDGE_CURVE('',#1745,#1745,#1502,.T.);
#2143=EDGE_CURVE('',#1746,#1746,#1503,.F.);
#2144=EDGE_CURVE('',#1747,#1748,#426,.T.);
#2145=EDGE_CURVE('',#1749,#1747,#1504,.F.);
#2146=EDGE_CURVE('',#1749,#1745,#427,.T.);
#2147=EDGE_CURVE('',#1750,#1749,#1505,.F.);
#2148=EDGE_CURVE('',#1751,#1750,#428,.F.);
#2149=EDGE_CURVE('',#1752,#1751,#1506,.T.);
#2150=EDGE_CURVE('',#1753,#1752,#429,.T.);
#2151=EDGE_CURVE('',#1754,#1753,#1507,.F.);
#2152=EDGE_CURVE('',#1755,#1754,#430,.F.);
#2153=EDGE_CURVE('',#1748,#1755,#1508,.T.);
#2154=EDGE_CURVE('',#1756,#1756,#1509,.T.);
#2155=EDGE_CURVE('',#1752,#1751,#431,.T.);
#2156=EDGE_CURVE('',#1755,#1748,#432,.T.);
#2157=EDGE_CURVE('',#1757,#1758,#1510,.T.);
#2158=EDGE_CURVE('',#1758,#1757,#1511,.T.);
#2159=EDGE_CURVE('',#1758,#1756,#433,.T.);
#2160=EDGE_CURVE('',#1757,#1759,#434,.T.);
#2161=EDGE_CURVE('',#1722,#1759,#1512,.T.);
#2162=EDGE_CURVE('',#1728,#1721,#1513,.T.);
#2163=EDGE_CURVE('',#1731,#1729,#1514,.T.);
#2164=EDGE_CURVE('',#1725,#1730,#1515,.T.);
#2165=EDGE_CURVE('',#1759,#1726,#1516,.T.);
#2166=EDGE_CURVE('',#1754,#1747,#435,.T.);
#2167=EDGE_CURVE('',#1753,#1750,#436,.T.);
#2168=EDGE_CURVE('',#1760,#1760,#1517,.F.);
#2169=EDGE_CURVE('',#1746,#1760,#437,.T.);
#2170=EDGE_CURVE('',#1738,#1742,#1518,.F.);
#2171=EDGE_CURVE('',#1741,#1733,#1519,.F.);
#2172=EDGE_CURVE('',#1737,#1761,#438,.T.);
#2173=EDGE_CURVE('',#1761,#1762,#1520,.T.);
#2174=EDGE_CURVE('',#1762,#1735,#439,.T.);
#2175=EDGE_CURVE('',#1734,#1739,#1521,.T.);
#2176=EDGE_CURVE('',#1740,#1763,#440,.T.);
#2177=EDGE_CURVE('',#1763,#1764,#1522,.T.);
#2178=EDGE_CURVE('',#1764,#1744,#441,.T.);
#2179=EDGE_CURVE('',#1743,#1736,#1523,.T.);
#2180=EDGE_CURVE('',#1764,#1765,#79,.T.);
#2181=EDGE_CURVE('',#1765,#1726,#442,.T.);
#2182=EDGE_CURVE('',#1766,#1722,#443,.T.);
#2183=EDGE_CURVE('',#1766,#1763,#80,.T.);
#2184=EDGE_CURVE('',#1765,#1766,#1524,.F.);
#2185=EDGE_CURVE('',#1762,#1767,#81,.T.);
#2186=EDGE_CURVE('',#1767,#1729,#444,.T.);
#2187=EDGE_CURVE('',#1768,#1731,#445,.T.);
#2188=EDGE_CURVE('',#1768,#1761,#82,.T.);
#2189=EDGE_CURVE('',#1767,#1768,#1525,.F.);
#2190=EDGE_CURVE('',#1769,#1770,#1526,.T.);
#2191=EDGE_CURVE('',#1769,#1771,#446,.T.);
#2192=EDGE_CURVE('',#1771,#1770,#447,.T.);
#2193=EDGE_CURVE('',#1770,#1772,#1527,.T.);
#2194=EDGE_CURVE('',#1770,#1773,#448,.T.);
#2195=EDGE_CURVE('',#1773,#1772,#449,.T.);
#2196=EDGE_CURVE('',#1772,#1774,#1528,.T.);
#2197=EDGE_CURVE('',#1772,#1775,#450,.T.);
#2198=EDGE_CURVE('',#1775,#1774,#451,.T.);
#2199=EDGE_CURVE('',#1776,#1776,#1529,.T.);
#2200=EDGE_CURVE('',#1777,#1777,#1530,.T.);
#2201=EDGE_CURVE('',#1778,#1779,#452,.T.);
#2202=EDGE_CURVE('',#1780,#1778,#453,.T.);
#2203=EDGE_CURVE('',#1781,#1780,#454,.T.);
#2204=EDGE_CURVE('',#1779,#1781,#455,.T.);
#2205=EDGE_CURVE('',#1782,#1782,#1531,.T.);
#2206=EDGE_CURVE('',#1782,#1777,#456,.T.);
#2207=EDGE_CURVE('',#1783,#1783,#1532,.T.);
#2208=EDGE_CURVE('',#1784,#1784,#1533,.F.);
#2209=EDGE_CURVE('',#1784,#1783,#457,.T.);
#2210=EDGE_CURVE('',#1785,#1786,#1343,.T.);
#2211=EDGE_CURVE('',#1786,#1785,#1344,.T.);
#2212=EDGE_CURVE('',#1787,#1788,#1345,.T.);
#2213=EDGE_CURVE('',#1788,#1787,#1346,.T.);
#2214=EDGE_CURVE('',#1786,#1788,#458,.T.);
#2215=EDGE_CURVE('',#1776,#1784,#1534,.T.);
#2216=EDGE_CURVE('',#1771,#1779,#459,.T.);
#2217=EDGE_CURVE('',#1789,#1769,#460,.T.);
#2218=EDGE_CURVE('',#1789,#1778,#461,.T.);
#2219=EDGE_CURVE('',#1773,#1781,#462,.T.);
#2220=EDGE_CURVE('',#1775,#1780,#463,.T.);
#2221=EDGE_CURVE('',#1774,#1789,#464,.T.);
#2222=EDGE_CURVE('',#1774,#1769,#1535,.T.);
#2223=EDGE_CURVE('',#1769,#1790,#465,.T.);
#2224=EDGE_CURVE('',#1790,#1790,#1536,.T.);
#2225=EDGE_CURVE('',#1791,#1791,#1537,.T.);
#2226=EDGE_CURVE('',#1792,#1792,#1538,.T.);
#2227=EDGE_CURVE('',#1793,#1793,#1539,.T.);
#2228=EDGE_CURVE('',#1794,#1794,#1540,.T.);
#2229=EDGE_CURVE('',#1793,#1795,#466,.T.);
#2230=EDGE_CURVE('',#1795,#1796,#1347,.T.);
#2231=EDGE_CURVE('',#1796,#1797,#1348,.T.);
#2232=EDGE_CURVE('',#1797,#1798,#1349,.T.);
#2233=EDGE_CURVE('',#1798,#1791,#467,.T.);
#2234=EDGE_CURVE('',#1798,#1795,#1350,.T.);
#2235=EDGE_CURVE('',#1799,#1800,#1351,.T.);
#2236=EDGE_CURVE('',#1800,#1799,#1352,.T.);
#2237=EDGE_CURVE('',#1792,#1801,#468,.T.);
#2238=EDGE_CURVE('',#1802,#1801,#1353,.T.);
#2239=EDGE_CURVE('',#1803,#1802,#1354,.T.);
#2240=EDGE_CURVE('',#1804,#1803,#1355,.T.);
#2241=EDGE_CURVE('',#1804,#1794,#469,.T.);
#2242=EDGE_CURVE('',#1801,#1804,#1356,.T.);
#2243=EDGE_CURVE('',#1805,#1806,#1357,.T.);
#2244=EDGE_CURVE('',#1806,#1805,#1358,.T.);
#2245=EDGE_CURVE('',#1802,#1797,#470,.T.);
#2246=EDGE_CURVE('',#1800,#1806,#471,.T.);
#2247=EDGE_CURVE('',#1807,#1807,#1541,.T.);
#2248=EDGE_CURVE('',#1807,#1808,#472,.T.);
#2249=EDGE_CURVE('',#1808,#1808,#1542,.T.);
#2250=EDGE_CURVE('',#1809,#1809,#1543,.T.);
#2251=EDGE_CURVE('',#1810,#1810,#1544,.T.);
#2252=EDGE_CURVE('',#1810,#1811,#473,.T.);
#2253=EDGE_CURVE('',#1811,#1812,#1545,.T.);
#2254=EDGE_CURVE('',#1812,#1811,#1546,.T.);
#2255=EDGE_CURVE('',#1813,#1814,#1547,.T.);
#2256=EDGE_CURVE('',#1814,#1813,#1548,.T.);
#2257=EDGE_CURVE('',#1813,#1812,#474,.T.);
#2258=EDGE_CURVE('',#1814,#1815,#475,.T.);
#2259=EDGE_CURVE('',#1815,#1815,#1549,.T.);
#2260=EDGE_CURVE('',#1816,#1816,#1550,.T.);
#2261=EDGE_CURVE('',#1817,#1817,#1551,.T.);
#2262=EDGE_CURVE('',#1817,#1816,#476,.T.);
#2263=EDGE_CURVE('',#1818,#1818,#1552,.T.);
#2264=EDGE_CURVE('',#1818,#1819,#477,.T.);
#2265=EDGE_CURVE('',#1819,#1819,#1553,.T.);
#2266=EDGE_CURVE('',#1820,#1820,#1554,.T.);
#2267=EDGE_CURVE('',#1821,#1821,#1555,.T.);
#2268=EDGE_CURVE('',#1822,#1822,#1556,.T.);
#2269=EDGE_CURVE('',#1823,#1823,#1557,.T.);
#2270=EDGE_CURVE('',#1824,#1824,#1558,.T.);
#2271=EDGE_CURVE('',#1820,#1825,#478,.T.);
#2272=EDGE_CURVE('',#1825,#1825,#1559,.T.);
#2273=EDGE_CURVE('',#1826,#1826,#1560,.T.);
#2274=EDGE_CURVE('',#1827,#1827,#1561,.T.);
#2275=EDGE_CURVE('',#1828,#1828,#1562,.T.);
#2276=EDGE_CURVE('',#1829,#1829,#1563,.T.);
#2277=EDGE_CURVE('',#1830,#1830,#1564,.T.);
#2278=EDGE_CURVE('',#1830,#1809,#479,.T.);
#2279=EDGE_CURVE('',#1824,#1829,#480,.T.);
#2280=EDGE_CURVE('',#1823,#1828,#481,.T.);
#2281=EDGE_CURVE('',#1822,#1827,#482,.T.);
#2282=EDGE_CURVE('',#1821,#1826,#483,.T.);
#2283=EDGE_CURVE('',#1831,#1831,#1565,.T.);
#2284=EDGE_CURVE('',#1831,#1832,#484,.T.);
#2285=EDGE_CURVE('',#1832,#1832,#1566,.T.);
#2286=EDGE_CURVE('',#1833,#1833,#1567,.T.);
#2287=EDGE_CURVE('',#1834,#1834,#1568,.T.);
#2288=EDGE_CURVE('',#1834,#1833,#485,.T.);
#2289=EDGE_CURVE('',#1835,#1835,#1569,.T.);
#2290=EDGE_CURVE('',#1836,#1836,#1570,.T.);
#2291=EDGE_CURVE('',#1836,#1835,#486,.T.);
#2292=EDGE_CURVE('',#1832,#1836,#487,.T.);
#2293=EDGE_CURVE('',#1837,#1838,#488,.T.);
#2294=EDGE_CURVE('',#1837,#1839,#1359,.T.);
#2295=EDGE_CURVE('',#1839,#1840,#1360,.T.);
#2296=EDGE_CURVE('',#1840,#1841,#489,.T.);
#2297=EDGE_CURVE('',#1841,#1838,#490,.T.);
#2298=EDGE_CURVE('',#1842,#1843,#491,.T.);
#2299=EDGE_CURVE('',#1842,#1844,#1361,.T.);
#2300=EDGE_CURVE('',#1844,#1837,#1362,.T.);
#2301=EDGE_CURVE('',#1838,#1843,#492,.T.);
#2302=EDGE_CURVE('',#1845,#1846,#1363,.T.);
#2303=EDGE_CURVE('',#1846,#1842,#1364,.T.);
#2304=EDGE_CURVE('',#1843,#1847,#493,.T.);
#2305=EDGE_CURVE('',#1845,#1847,#494,.T.);
#2306=EDGE_CURVE('',#1848,#1849,#495,.T.);
#2307=EDGE_CURVE('',#1848,#1850,#1365,.T.);
#2308=EDGE_CURVE('',#1850,#1845,#1366,.T.);
#2309=EDGE_CURVE('',#1847,#1849,#496,.T.);
#2310=EDGE_CURVE('',#1851,#1852,#497,.T.);
#2311=EDGE_CURVE('',#1851,#1853,#1367,.T.);
#2312=EDGE_CURVE('',#1853,#1848,#1368,.T.);
#2313=EDGE_CURVE('',#1849,#1852,#498,.T.);
#2314=EDGE_CURVE('',#1840,#1854,#1369,.T.);
#2315=EDGE_CURVE('',#1854,#1851,#1370,.T.);
#2316=EDGE_CURVE('',#1852,#1841,#499,.T.);
#2317=EDGE_CURVE('',#1855,#1855,#1571,.T.);
#2318=EDGE_CURVE('',#1856,#1856,#1572,.T.);
#2319=EDGE_CURVE('',#1856,#1855,#500,.T.);
#2320=EDGE_CURVE('',#1857,#1857,#1573,.T.);
#2321=EDGE_CURVE('',#1839,#1854,#1574,.T.);
#2322=EDGE_CURVE('',#1844,#1839,#1575,.T.);
#2323=EDGE_CURVE('',#1846,#1844,#1576,.T.);
#2324=EDGE_CURVE('',#1850,#1846,#1577,.T.);
#2325=EDGE_CURVE('',#1853,#1850,#1578,.T.);
#2326=EDGE_CURVE('',#1854,#1853,#1579,.T.);
#2327=EDGE_CURVE('',#1858,#1858,#1580,.T.);
#2328=EDGE_CURVE('',#1859,#1859,#1581,.T.);
#2329=EDGE_CURVE('',#1854,#1858,#501,.T.);
#2330=EDGE_CURVE('',#1860,#1860,#1582,.T.);
#2331=EDGE_CURVE('',#1860,#1857,#502,.T.);
#2332=EDGE_CURVE('',#1861,#1861,#1583,.T.);
#2333=EDGE_CURVE('',#1861,#1859,#503,.T.);
#2334=EDGE_CURVE('',#1862,#1863,#504,.T.);
#2335=EDGE_CURVE('',#1863,#1864,#1371,.T.);
#2336=EDGE_CURVE('',#1864,#1865,#505,.T.);
#2337=EDGE_CURVE('',#1865,#1866,#1372,.T.);
#2338=EDGE_CURVE('',#1866,#1867,#506,.T.);
#2339=EDGE_CURVE('',#1867,#1862,#1373,.T.);
#2340=EDGE_CURVE('',#1868,#1869,#507,.T.);
#2341=EDGE_CURVE('',#1868,#1870,#1374,.T.);
#2342=EDGE_CURVE('',#1871,#1870,#508,.T.);
#2343=EDGE_CURVE('',#1871,#1872,#1375,.T.);
#2344=EDGE_CURVE('',#1873,#1872,#509,.T.);
#2345=EDGE_CURVE('',#1873,#1869,#1376,.T.);
#2346=EDGE_CURVE('',#1869,#1865,#1584,.T.);
#2347=EDGE_CURVE('',#1864,#1874,#1377,.T.);
#2348=EDGE_CURVE('',#1874,#1875,#1585,.T.);
#2349=EDGE_CURVE('',#1875,#1868,#1378,.T.);
#2350=EDGE_CURVE('',#1876,#1877,#510,.T.);
#2351=EDGE_CURVE('',#1876,#1878,#1586,.T.);
#2352=EDGE_CURVE('',#1878,#1879,#511,.T.);
#2353=EDGE_CURVE('',#1879,#1880,#1379,.T.);
#2354=EDGE_CURVE('',#1880,#1881,#1587,.T.);
#2355=EDGE_CURVE('',#1881,#1882,#1588,.T.);
#2356=EDGE_CURVE('',#1882,#1877,#1380,.T.);
#2357=EDGE_CURVE('',#1883,#1884,#512,.T.);
#2358=EDGE_CURVE('',#1883,#1885,#1589,.T.);
#2359=EDGE_CURVE('',#1885,#1886,#513,.T.);
#2360=EDGE_CURVE('',#1886,#1887,#1381,.T.);
#2361=EDGE_CURVE('',#1887,#1888,#1590,.T.);
#2362=EDGE_CURVE('',#1888,#1884,#1382,.T.);
#2363=EDGE_CURVE('',#1889,#1890,#514,.T.);
#2364=EDGE_CURVE('',#1890,#1891,#1591,.T.);
#2365=EDGE_CURVE('',#1892,#1891,#515,.T.);
#2366=EDGE_CURVE('',#1892,#1893,#1383,.T.);
#2367=EDGE_CURVE('',#1893,#1894,#1592,.T.);
#2368=EDGE_CURVE('',#1894,#1895,#1593,.T.);
#2369=EDGE_CURVE('',#1895,#1889,#1384,.T.);
#2370=EDGE_CURVE('',#1862,#1871,#1594,.T.);
#2371=EDGE_CURVE('',#1870,#1896,#1385,.T.);
#2372=EDGE_CURVE('',#1896,#1897,#1595,.T.);
#2373=EDGE_CURVE('',#1897,#1863,#1386,.T.);
#2374=EDGE_CURVE('',#1898,#1899,#516,.T.);
#2375=EDGE_CURVE('',#1898,#1900,#1596,.T.);
#2376=EDGE_CURVE('',#1900,#1901,#517,.T.);
#2377=EDGE_CURVE('',#1901,#1902,#1387,.T.);
#2378=EDGE_CURVE('',#1902,#1903,#1597,.T.);
#2379=EDGE_CURVE('',#1903,#1899,#1388,.T.);
#2380=EDGE_CURVE('',#1884,#1904,#1389,.T.);
#2381=EDGE_CURVE('',#1904,#1905,#518,.T.);
#2382=EDGE_CURVE('',#1905,#1906,#1390,.T.);
#2383=EDGE_CURVE('',#1906,#1907,#519,.F.);
#2384=EDGE_CURVE('',#1907,#1883,#1391,.T.);
#2385=EDGE_CURVE('',#1908,#1909,#520,.T.);
#2386=EDGE_CURVE('',#1908,#1886,#1392,.T.);
#2387=EDGE_CURVE('',#1885,#1910,#1393,.T.);
#2388=EDGE_CURVE('',#1911,#1910,#521,.F.);
#2389=EDGE_CURVE('',#1911,#1909,#1394,.T.);
#2390=EDGE_CURVE('',#1877,#1892,#1395,.T.);
#2391=EDGE_CURVE('',#1891,#1912,#1396,.T.);
#2392=EDGE_CURVE('',#1912,#1913,#522,.F.);
#2393=EDGE_CURVE('',#1913,#1876,#1397,.T.);
#2394=EDGE_CURVE('',#1889,#1879,#1398,.T.);
#2395=EDGE_CURVE('',#1878,#1914,#1399,.T.);
#2396=EDGE_CURVE('',#1915,#1914,#523,.F.);
#2397=EDGE_CURVE('',#1915,#1890,#1400,.T.);
#2398=EDGE_CURVE('',#1899,#1916,#1401,.T.);
#2399=EDGE_CURVE('',#1916,#1917,#524,.T.);
#2400=EDGE_CURVE('',#1917,#1918,#1402,.T.);
#2401=EDGE_CURVE('',#1918,#1919,#525,.T.);
#2402=EDGE_CURVE('',#1919,#1898,#1403,.T.);
#2403=EDGE_CURVE('',#1920,#1921,#526,.T.);
#2404=EDGE_CURVE('',#1920,#1901,#1404,.T.);
#2405=EDGE_CURVE('',#1900,#1922,#1405,.T.);
#2406=EDGE_CURVE('',#1923,#1922,#527,.T.);
#2407=EDGE_CURVE('',#1923,#1921,#1406,.T.);
#2408=EDGE_CURVE('',#1894,#1881,#1598,.T.);
#2409=EDGE_CURVE('',#1893,#1924,#1407,.T.);
#2410=EDGE_CURVE('',#1924,#1925,#1599,.T.);
#2411=EDGE_CURVE('',#1925,#1926,#1408,.T.);
#2412=EDGE_CURVE('',#1927,#1926,#1600,.T.);
#2413=EDGE_CURVE('',#1927,#1928,#1409,.T.);
#2414=EDGE_CURVE('',#1928,#1929,#1601,.T.);
#2415=EDGE_CURVE('',#1929,#1903,#1410,.T.);
#2416=EDGE_CURVE('',#1902,#1930,#1411,.T.);
#2417=EDGE_CURVE('',#1930,#1931,#1602,.T.);
#2418=EDGE_CURVE('',#1931,#1897,#1412,.T.);
#2419=EDGE_CURVE('',#1896,#1932,#1413,.T.);
#2420=EDGE_CURVE('',#1932,#1933,#1603,.T.);
#2421=EDGE_CURVE('',#1933,#1895,#1414,.T.);
#2422=EDGE_CURVE('',#1880,#1933,#1415,.T.);
#2423=EDGE_CURVE('',#1932,#1875,#1416,.T.);
#2424=EDGE_CURVE('',#1874,#1931,#1417,.T.);
#2425=EDGE_CURVE('',#1930,#1934,#1418,.T.);
#2426=EDGE_CURVE('',#1935,#1934,#1604,.T.);
#2427=EDGE_CURVE('',#1935,#1929,#1419,.T.);
#2428=EDGE_CURVE('',#1928,#1888,#1420,.T.);
#2429=EDGE_CURVE('',#1887,#1925,#1421,.T.);
#2430=EDGE_CURVE('',#1924,#1882,#1422,.T.);
#2431=EDGE_CURVE('',#1921,#1917,#1605,.T.);
#2432=EDGE_CURVE('',#1916,#1935,#1423,.T.);
#2433=EDGE_CURVE('',#1934,#1920,#1424,.T.);
#2434=EDGE_CURVE('',#1909,#1905,#1606,.T.);
#2435=EDGE_CURVE('',#1904,#1927,#1425,.T.);
#2436=EDGE_CURVE('',#1926,#1908,#1426,.T.);
#2437=EDGE_CURVE('',#1936,#1936,#1607,.T.);
#2438=EDGE_CURVE('',#1936,#1937,#528,.T.);
#2439=EDGE_CURVE('',#1937,#1915,#1608,.F.);
#2440=EDGE_CURVE('',#1914,#1938,#1609,.F.);
#2441=EDGE_CURVE('',#1938,#1939,#529,.T.);
#2442=EDGE_CURVE('',#1939,#1939,#1610,.T.);
#2443=EDGE_CURVE('',#1938,#1913,#1611,.F.);
#2444=EDGE_CURVE('',#1912,#1937,#1612,.F.);
#2445=EDGE_CURVE('',#1910,#1907,#1613,.F.);
#2446=EDGE_CURVE('',#1906,#1911,#1614,.F.);
#2447=EDGE_CURVE('',#1918,#1923,#1615,.F.);
#2448=EDGE_CURVE('',#1922,#1919,#1616,.F.);
#2449=EDGE_CURVE('',#1872,#1867,#1617,.F.);
#2450=EDGE_CURVE('',#1866,#1873,#1618,.F.);
#2451=EDGE_CURVE('',#1940,#1941,#530,.T.);
#2452=EDGE_CURVE('',#1941,#1942,#531,.T.);
#2453=EDGE_CURVE('',#1942,#1943,#532,.T.);
#2454=EDGE_CURVE('',#1943,#1940,#533,.T.);
#2455=EDGE_CURVE('',#1944,#1945,#534,.T.);
#2456=EDGE_CURVE('',#1946,#1944,#535,.T.);
#2457=EDGE_CURVE('',#1947,#1946,#536,.T.);
#2458=EDGE_CURVE('',#1945,#1947,#537,.T.);
#2459=EDGE_CURVE('',#1941,#1944,#538,.T.);
#2460=EDGE_CURVE('',#1940,#1946,#539,.T.);
#2461=EDGE_CURVE('',#1943,#1947,#540,.T.);
#2462=EDGE_CURVE('',#1942,#1945,#541,.T.);
#2463=EDGE_CURVE('',#1948,#1949,#83,.T.);
#2464=EDGE_CURVE('',#1950,#1948,#542,.T.);
#2465=EDGE_CURVE('',#1951,#1950,#84,.T.);
#2466=EDGE_CURVE('',#1952,#1951,#85,.T.);
#2467=EDGE_CURVE('',#1952,#1953,#543,.T.);
#2468=EDGE_CURVE('',#1949,#1953,#86,.T.);
#2469=EDGE_CURVE('',#1954,#1955,#87,.T.);
#2470=EDGE_CURVE('',#1956,#1954,#544,.T.);
#2471=EDGE_CURVE('',#1957,#1956,#88,.T.);
#2472=EDGE_CURVE('',#1950,#1957,#89,.T.);
#2473=EDGE_CURVE('',#1955,#1948,#90,.T.);
#2474=EDGE_CURVE('',#1958,#1959,#91,.T.);
#2475=EDGE_CURVE('',#1960,#1958,#545,.T.);
#2476=EDGE_CURVE('',#1961,#1960,#92,.T.);
#2477=EDGE_CURVE('',#1956,#1961,#93,.T.);
#2478=EDGE_CURVE('',#1959,#1954,#94,.T.);
#2479=EDGE_CURVE('',#1962,#1963,#95,.T.);
#2480=EDGE_CURVE('',#1964,#1962,#546,.T.);
#2481=EDGE_CURVE('',#1965,#1964,#96,.T.);
#2482=EDGE_CURVE('',#1960,#1965,#97,.T.);
#2483=EDGE_CURVE('',#1963,#1958,#98,.T.);
#2484=EDGE_CURVE('',#1966,#1967,#99,.T.);
#2485=EDGE_CURVE('',#1968,#1966,#547,.T.);
#2486=EDGE_CURVE('',#1969,#1968,#100,.T.);
#2487=EDGE_CURVE('',#1964,#1969,#101,.T.);
#2488=EDGE_CURVE('',#1967,#1962,#102,.T.);
#2489=EDGE_CURVE('',#1953,#1970,#103,.T.);
#2490=EDGE_CURVE('',#1971,#1952,#104,.T.);
#2491=EDGE_CURVE('',#1968,#1971,#105,.T.);
#2492=EDGE_CURVE('',#1970,#1966,#106,.T.);
#2493=EDGE_CURVE('',#1970,#1949,#1619,.T.);
#2494=EDGE_CURVE('',#1967,#1970,#1620,.T.);
#2495=EDGE_CURVE('',#1963,#1967,#1621,.T.);
#2496=EDGE_CURVE('',#1959,#1963,#1622,.T.);
#2497=EDGE_CURVE('',#1959,#1955,#1623,.T.);
#2498=EDGE_CURVE('',#1949,#1955,#1624,.T.);
#2499=EDGE_CURVE('',#1972,#1972,#1625,.T.);
#2500=EDGE_CURVE('',#1969,#1971,#1626,.T.);
#2501=EDGE_CURVE('',#1971,#1951,#1627,.T.);
#2502=EDGE_CURVE('',#1951,#1957,#1628,.T.);
#2503=EDGE_CURVE('',#1957,#1961,#1629,.T.);
#2504=EDGE_CURVE('',#1961,#1965,#1630,.T.);
#2505=EDGE_CURVE('',#1965,#1969,#1631,.T.);
#2506=EDGE_CURVE('',#1973,#1973,#1632,.T.);
#2507=EDGE_CURVE('',#1973,#1972,#548,.T.);
#2508=EDGE_CURVE('',#1974,#1975,#107,.T.);
#2509=EDGE_CURVE('',#1974,#1976,#549,.T.);
#2510=EDGE_CURVE('',#1976,#1977,#550,.T.);
#2511=EDGE_CURVE('',#1978,#1977,#551,.T.);
#2512=EDGE_CURVE('',#1975,#1978,#108,.T.);
#2513=EDGE_CURVE('',#1978,#1979,#109,.T.);
#2514=EDGE_CURVE('',#1977,#1980,#552,.T.);
#2515=EDGE_CURVE('',#1981,#1980,#553,.T.);
#2516=EDGE_CURVE('',#1979,#1981,#110,.T.);
#2517=EDGE_CURVE('',#1981,#1982,#111,.T.);
#2518=EDGE_CURVE('',#1980,#1983,#554,.T.);
#2519=EDGE_CURVE('',#1984,#1983,#555,.T.);
#2520=EDGE_CURVE('',#1982,#1984,#112,.T.);
#2521=EDGE_CURVE('',#1984,#1985,#113,.T.);
#2522=EDGE_CURVE('',#1983,#1986,#556,.T.);
#2523=EDGE_CURVE('',#1987,#1986,#557,.T.);
#2524=EDGE_CURVE('',#1985,#1987,#114,.T.);
#2525=EDGE_CURVE('',#1987,#1988,#115,.T.);
#2526=EDGE_CURVE('',#1986,#1989,#558,.T.);
#2527=EDGE_CURVE('',#1990,#1989,#559,.T.);
#2528=EDGE_CURVE('',#1988,#1990,#116,.T.);
#2529=EDGE_CURVE('',#1990,#1991,#117,.T.);
#2530=EDGE_CURVE('',#1989,#1976,#560,.T.);
#2531=EDGE_CURVE('',#1991,#1974,#118,.T.);
#2532=EDGE_CURVE('',#1992,#1992,#1633,.T.);
#2533=EDGE_CURVE('',#1992,#1993,#561,.T.);
#2534=EDGE_CURVE('',#1993,#1993,#1634,.T.);
#2535=EDGE_CURVE('',#1988,#1991,#1635,.T.);
#2536=EDGE_CURVE('',#1985,#1988,#1636,.T.);
#2537=EDGE_CURVE('',#1982,#1985,#1637,.T.);
#2538=EDGE_CURVE('',#1979,#1982,#1638,.T.);
#2539=EDGE_CURVE('',#1975,#1979,#1639,.T.);
#2540=EDGE_CURVE('',#1991,#1975,#1640,.T.);
#2541=ORIENTED_EDGE('',*,*,#1994,.F.);
#2542=ORIENTED_EDGE('',*,*,#1995,.T.);
#2543=ORIENTED_EDGE('',*,*,#1996,.T.);
#2544=ORIENTED_EDGE('',*,*,#1997,.T.);
#2545=ORIENTED_EDGE('',*,*,#1998,.T.);
#2546=ORIENTED_EDGE('',*,*,#1999,.T.);
#2547=ORIENTED_EDGE('',*,*,#2000,.T.);
#2548=ORIENTED_EDGE('',*,*,#2001,.T.);
#2549=ORIENTED_EDGE('',*,*,#2002,.T.);
#2550=ORIENTED_EDGE('',*,*,#2003,.T.);
#2551=ORIENTED_EDGE('',*,*,#2004,.F.);
#2552=ORIENTED_EDGE('',*,*,#2005,.T.);
#2553=ORIENTED_EDGE('',*,*,#2004,.T.);
#2554=ORIENTED_EDGE('',*,*,#2006,.T.);
#2555=ORIENTED_EDGE('',*,*,#2007,.T.);
#2556=ORIENTED_EDGE('',*,*,#2008,.T.);
#2557=ORIENTED_EDGE('',*,*,#2009,.T.);
#2558=ORIENTED_EDGE('',*,*,#2010,.F.);
#2559=ORIENTED_EDGE('',*,*,#2011,.F.);
#2560=ORIENTED_EDGE('',*,*,#2012,.T.);
#2561=ORIENTED_EDGE('',*,*,#2013,.T.);
#2562=ORIENTED_EDGE('',*,*,#2014,.T.);
#2563=ORIENTED_EDGE('',*,*,#2015,.T.);
#2564=ORIENTED_EDGE('',*,*,#2016,.T.);
#2565=ORIENTED_EDGE('',*,*,#2017,.T.);
#2566=ORIENTED_EDGE('',*,*,#2012,.F.);
#2567=ORIENTED_EDGE('',*,*,#1994,.T.);
#2568=ORIENTED_EDGE('',*,*,#2018,.T.);
#2569=ORIENTED_EDGE('',*,*,#2019,.F.);
#2570=ORIENTED_EDGE('',*,*,#2013,.F.);
#2571=ORIENTED_EDGE('',*,*,#2017,.F.);
#2572=ORIENTED_EDGE('',*,*,#2020,.F.);
#2573=ORIENTED_EDGE('',*,*,#2021,.T.);
#2574=ORIENTED_EDGE('',*,*,#2022,.F.);
#2575=ORIENTED_EDGE('',*,*,#2023,.F.);
#2576=ORIENTED_EDGE('',*,*,#2024,.F.);
#2577=ORIENTED_EDGE('',*,*,#2025,.F.);
#2578=ORIENTED_EDGE('',*,*,#2026,.T.);
#2579=ORIENTED_EDGE('',*,*,#2027,.T.);
#2580=ORIENTED_EDGE('',*,*,#2028,.T.);
#2581=ORIENTED_EDGE('',*,*,#2029,.T.);
#2582=ORIENTED_EDGE('',*,*,#2026,.F.);
#2583=ORIENTED_EDGE('',*,*,#2029,.F.);
#2584=ORIENTED_EDGE('',*,*,#2027,.F.);
#2585=ORIENTED_EDGE('',*,*,#2028,.F.);
#2586=ORIENTED_EDGE('',*,*,#2030,.T.);
#2587=ORIENTED_EDGE('',*,*,#2031,.T.);
#2588=ORIENTED_EDGE('',*,*,#2030,.F.);
#2589=ORIENTED_EDGE('',*,*,#2031,.F.);
#2590=ORIENTED_EDGE('',*,*,#2032,.T.);
#2591=ORIENTED_EDGE('',*,*,#2032,.F.);
#2592=ORIENTED_EDGE('',*,*,#2033,.T.);
#2593=ORIENTED_EDGE('',*,*,#2034,.T.);
#2594=ORIENTED_EDGE('',*,*,#2033,.F.);
#2595=ORIENTED_EDGE('',*,*,#2035,.T.);
#2596=ORIENTED_EDGE('',*,*,#2034,.F.);
#2597=ORIENTED_EDGE('',*,*,#2036,.F.);
#2598=ORIENTED_EDGE('',*,*,#2037,.F.);
#2599=ORIENTED_EDGE('',*,*,#2038,.F.);
#2600=ORIENTED_EDGE('',*,*,#2039,.F.);
#2601=ORIENTED_EDGE('',*,*,#2035,.F.);
#2602=ORIENTED_EDGE('',*,*,#2040,.T.);
#2603=ORIENTED_EDGE('',*,*,#2041,.T.);
#2604=ORIENTED_EDGE('',*,*,#2042,.T.);
#2605=ORIENTED_EDGE('',*,*,#2040,.F.);
#2606=ORIENTED_EDGE('',*,*,#2043,.T.);
#2607=ORIENTED_EDGE('',*,*,#2044,.T.);
#2608=ORIENTED_EDGE('',*,*,#2045,.T.);
#2609=ORIENTED_EDGE('',*,*,#2046,.T.);
#2610=ORIENTED_EDGE('',*,*,#2047,.T.);
#2611=ORIENTED_EDGE('',*,*,#2048,.T.);
#2612=ORIENTED_EDGE('',*,*,#2048,.F.);
#2613=ORIENTED_EDGE('',*,*,#2049,.T.);
#2614=ORIENTED_EDGE('',*,*,#2050,.T.);
#2615=ORIENTED_EDGE('',*,*,#2051,.T.);
#2616=ORIENTED_EDGE('',*,*,#2049,.F.);
#2617=ORIENTED_EDGE('',*,*,#2050,.F.);
#2618=ORIENTED_EDGE('',*,*,#2051,.F.);
#2619=ORIENTED_EDGE('',*,*,#2052,.T.);
#2620=ORIENTED_EDGE('',*,*,#2053,.T.);
#2621=ORIENTED_EDGE('',*,*,#2052,.F.);
#2622=ORIENTED_EDGE('',*,*,#2054,.T.);
#2623=ORIENTED_EDGE('',*,*,#2053,.F.);
#2624=ORIENTED_EDGE('',*,*,#2054,.F.);
#2625=ORIENTED_EDGE('',*,*,#2055,.T.);
#2626=ORIENTED_EDGE('',*,*,#2056,.T.);
#2627=ORIENTED_EDGE('',*,*,#2057,.T.);
#2628=ORIENTED_EDGE('',*,*,#2008,.F.);
#2629=ORIENTED_EDGE('',*,*,#2058,.T.);
#2630=ORIENTED_EDGE('',*,*,#2055,.F.);
#2631=ORIENTED_EDGE('',*,*,#2009,.F.);
#2632=ORIENTED_EDGE('',*,*,#2057,.F.);
#2633=ORIENTED_EDGE('',*,*,#2059,.T.);
#2634=ORIENTED_EDGE('',*,*,#2010,.T.);
#2635=ORIENTED_EDGE('',*,*,#2011,.T.);
#2636=ORIENTED_EDGE('',*,*,#2059,.F.);
#2637=ORIENTED_EDGE('',*,*,#2056,.F.);
#2638=ORIENTED_EDGE('',*,*,#2058,.F.);
#2639=ORIENTED_EDGE('',*,*,#2007,.F.);
#2640=ORIENTED_EDGE('',*,*,#2002,.F.);
#2641=ORIENTED_EDGE('',*,*,#2060,.T.);
#2642=ORIENTED_EDGE('',*,*,#1997,.F.);
#2643=ORIENTED_EDGE('',*,*,#2061,.T.);
#2644=ORIENTED_EDGE('',*,*,#2062,.T.);
#2645=ORIENTED_EDGE('',*,*,#2061,.F.);
#2646=ORIENTED_EDGE('',*,*,#1996,.F.);
#2647=ORIENTED_EDGE('',*,*,#2063,.T.);
#2648=ORIENTED_EDGE('',*,*,#2062,.F.);
#2649=ORIENTED_EDGE('',*,*,#2064,.T.);
#2650=ORIENTED_EDGE('',*,*,#2065,.T.);
#2651=ORIENTED_EDGE('',*,*,#2066,.T.);
#2652=ORIENTED_EDGE('',*,*,#2067,.T.);
#2653=ORIENTED_EDGE('',*,*,#2068,.T.);
#2654=ORIENTED_EDGE('',*,*,#2069,.T.);
#2655=ORIENTED_EDGE('',*,*,#2070,.T.);
#2656=ORIENTED_EDGE('',*,*,#2071,.T.);
#2657=ORIENTED_EDGE('',*,*,#2072,.T.);
#2658=ORIENTED_EDGE('',*,*,#2071,.F.);
#2659=ORIENTED_EDGE('',*,*,#2073,.T.);
#2660=ORIENTED_EDGE('',*,*,#2072,.F.);
#2661=ORIENTED_EDGE('',*,*,#2073,.F.);
#2662=ORIENTED_EDGE('',*,*,#2074,.T.);
#2663=ORIENTED_EDGE('',*,*,#2075,.T.);
#2664=ORIENTED_EDGE('',*,*,#2074,.F.);
#2665=ORIENTED_EDGE('',*,*,#2076,.T.);
#2666=ORIENTED_EDGE('',*,*,#2077,.T.);
#2667=ORIENTED_EDGE('',*,*,#2075,.F.);
#2668=ORIENTED_EDGE('',*,*,#2078,.T.);
#2669=ORIENTED_EDGE('',*,*,#2078,.F.);
#2670=ORIENTED_EDGE('',*,*,#2079,.T.);
#2671=ORIENTED_EDGE('',*,*,#2025,.T.);
#2672=ORIENTED_EDGE('',*,*,#2079,.F.);
#2673=ORIENTED_EDGE('',*,*,#2080,.F.);
#2674=ORIENTED_EDGE('',*,*,#2081,.T.);
#2675=ORIENTED_EDGE('',*,*,#2082,.T.);
#2676=ORIENTED_EDGE('',*,*,#2081,.F.);
#2677=ORIENTED_EDGE('',*,*,#2082,.F.);
#2678=ORIENTED_EDGE('',*,*,#2083,.F.);
#2679=ORIENTED_EDGE('',*,*,#2084,.F.);
#2680=ORIENTED_EDGE('',*,*,#2085,.F.);
#2681=ORIENTED_EDGE('',*,*,#2086,.F.);
#2682=ORIENTED_EDGE('',*,*,#2005,.F.);
#2683=ORIENTED_EDGE('',*,*,#2080,.T.);
#2684=ORIENTED_EDGE('',*,*,#2087,.F.);
#2685=ORIENTED_EDGE('',*,*,#2088,.F.);
#2686=ORIENTED_EDGE('',*,*,#2089,.F.);
#2687=ORIENTED_EDGE('',*,*,#2090,.F.);
#2688=ORIENTED_EDGE('',*,*,#2091,.F.);
#2689=ORIENTED_EDGE('',*,*,#1999,.F.);
#2690=ORIENTED_EDGE('',*,*,#2092,.T.);
#2691=ORIENTED_EDGE('',*,*,#2015,.F.);
#2692=ORIENTED_EDGE('',*,*,#2093,.F.);
#2693=ORIENTED_EDGE('',*,*,#2019,.T.);
#2694=ORIENTED_EDGE('',*,*,#2094,.T.);
#2695=ORIENTED_EDGE('',*,*,#2000,.F.);
#2696=ORIENTED_EDGE('',*,*,#2093,.T.);
#2697=ORIENTED_EDGE('',*,*,#2014,.F.);
#2698=ORIENTED_EDGE('',*,*,#2006,.F.);
#2699=ORIENTED_EDGE('',*,*,#2095,.T.);
#2700=ORIENTED_EDGE('',*,*,#2020,.T.);
#2701=ORIENTED_EDGE('',*,*,#2016,.F.);
#2702=ORIENTED_EDGE('',*,*,#2092,.F.);
#2703=ORIENTED_EDGE('',*,*,#2076,.F.);
#2704=ORIENTED_EDGE('',*,*,#2077,.F.);
#2705=ORIENTED_EDGE('',*,*,#2096,.T.);
#2706=ORIENTED_EDGE('',*,*,#2091,.T.);
#2707=ORIENTED_EDGE('',*,*,#2096,.F.);
#2708=ORIENTED_EDGE('',*,*,#2086,.T.);
#2709=ORIENTED_EDGE('',*,*,#2097,.T.);
#2710=ORIENTED_EDGE('',*,*,#2090,.T.);
#2711=ORIENTED_EDGE('',*,*,#2097,.F.);
#2712=ORIENTED_EDGE('',*,*,#2085,.T.);
#2713=ORIENTED_EDGE('',*,*,#2098,.T.);
#2714=ORIENTED_EDGE('',*,*,#2089,.T.);
#2715=ORIENTED_EDGE('',*,*,#2098,.F.);
#2716=ORIENTED_EDGE('',*,*,#2084,.T.);
#2717=ORIENTED_EDGE('',*,*,#2099,.T.);
#2718=ORIENTED_EDGE('',*,*,#2088,.T.);
#2719=ORIENTED_EDGE('',*,*,#2099,.F.);
#2720=ORIENTED_EDGE('',*,*,#2083,.T.);
#2721=ORIENTED_EDGE('',*,*,#2100,.T.);
#2722=ORIENTED_EDGE('',*,*,#2087,.T.);
#2723=ORIENTED_EDGE('',*,*,#2100,.F.);
#2724=ORIENTED_EDGE('',*,*,#2047,.F.);
#2725=ORIENTED_EDGE('',*,*,#2101,.T.);
#2726=ORIENTED_EDGE('',*,*,#2039,.T.);
#2727=ORIENTED_EDGE('',*,*,#2101,.F.);
#2728=ORIENTED_EDGE('',*,*,#2046,.F.);
#2729=ORIENTED_EDGE('',*,*,#2102,.T.);
#2730=ORIENTED_EDGE('',*,*,#2038,.T.);
#2731=ORIENTED_EDGE('',*,*,#2102,.F.);
#2732=ORIENTED_EDGE('',*,*,#2045,.F.);
#2733=ORIENTED_EDGE('',*,*,#2103,.T.);
#2734=ORIENTED_EDGE('',*,*,#2037,.T.);
#2735=ORIENTED_EDGE('',*,*,#2103,.F.);
#2736=ORIENTED_EDGE('',*,*,#2044,.F.);
#2737=ORIENTED_EDGE('',*,*,#2104,.T.);
#2738=ORIENTED_EDGE('',*,*,#2036,.T.);
#2739=ORIENTED_EDGE('',*,*,#2104,.F.);
#2740=ORIENTED_EDGE('',*,*,#2068,.F.);
#2741=ORIENTED_EDGE('',*,*,#2105,.T.);
#2742=ORIENTED_EDGE('',*,*,#2106,.T.);
#2743=ORIENTED_EDGE('',*,*,#2107,.T.);
#2744=ORIENTED_EDGE('',*,*,#2105,.F.);
#2745=ORIENTED_EDGE('',*,*,#2108,.T.);
#2746=ORIENTED_EDGE('',*,*,#2106,.F.);
#2747=ORIENTED_EDGE('',*,*,#2107,.F.);
#2748=ORIENTED_EDGE('',*,*,#2108,.F.);
#2749=ORIENTED_EDGE('',*,*,#2067,.F.);
#2750=ORIENTED_EDGE('',*,*,#2109,.T.);
#2751=ORIENTED_EDGE('',*,*,#2024,.T.);
#2752=ORIENTED_EDGE('',*,*,#2109,.F.);
#2753=ORIENTED_EDGE('',*,*,#2066,.F.);
#2754=ORIENTED_EDGE('',*,*,#2110,.T.);
#2755=ORIENTED_EDGE('',*,*,#2023,.T.);
#2756=ORIENTED_EDGE('',*,*,#2110,.F.);
#2757=ORIENTED_EDGE('',*,*,#2065,.F.);
#2758=ORIENTED_EDGE('',*,*,#2111,.T.);
#2759=ORIENTED_EDGE('',*,*,#2022,.T.);
#2760=ORIENTED_EDGE('',*,*,#2111,.F.);
#2761=ORIENTED_EDGE('',*,*,#2001,.F.);
#2762=ORIENTED_EDGE('',*,*,#2094,.F.);
#2763=ORIENTED_EDGE('',*,*,#2018,.F.);
#2764=ORIENTED_EDGE('',*,*,#1998,.F.);
#2765=ORIENTED_EDGE('',*,*,#2060,.F.);
#2766=ORIENTED_EDGE('',*,*,#2003,.F.);
#2767=ORIENTED_EDGE('',*,*,#2063,.F.);
#2768=ORIENTED_EDGE('',*,*,#1995,.F.);
#2769=ORIENTED_EDGE('',*,*,#2021,.F.);
#2770=ORIENTED_EDGE('',*,*,#2095,.F.);
#2771=ORIENTED_EDGE('',*,*,#2069,.F.);
#2772=ORIENTED_EDGE('',*,*,#2070,.F.);
#2773=ORIENTED_EDGE('',*,*,#2112,.T.);
#2774=ORIENTED_EDGE('',*,*,#2064,.F.);
#2775=ORIENTED_EDGE('',*,*,#2112,.F.);
#2776=ORIENTED_EDGE('',*,*,#2043,.F.);
#2777=ORIENTED_EDGE('',*,*,#2113,.T.);
#2778=ORIENTED_EDGE('',*,*,#2041,.F.);
#2779=ORIENTED_EDGE('',*,*,#2042,.F.);
#2780=ORIENTED_EDGE('',*,*,#2113,.F.);
#2781=ORIENTED_EDGE('',*,*,#2114,.T.);
#2782=ORIENTED_EDGE('',*,*,#2115,.F.);
#2783=ORIENTED_EDGE('',*,*,#2116,.F.);
#2784=ORIENTED_EDGE('',*,*,#2117,.F.);
#2785=ORIENTED_EDGE('',*,*,#2118,.F.);
#2786=ORIENTED_EDGE('',*,*,#2119,.T.);
#2787=ORIENTED_EDGE('',*,*,#2120,.F.);
#2788=ORIENTED_EDGE('',*,*,#2121,.F.);
#2789=ORIENTED_EDGE('',*,*,#2122,.T.);
#2790=ORIENTED_EDGE('',*,*,#2123,.T.);
#2791=ORIENTED_EDGE('',*,*,#2124,.F.);
#2792=ORIENTED_EDGE('',*,*,#2125,.F.);
#2793=ORIENTED_EDGE('',*,*,#2126,.F.);
#2794=ORIENTED_EDGE('',*,*,#2127,.T.);
#2795=ORIENTED_EDGE('',*,*,#2128,.F.);
#2796=ORIENTED_EDGE('',*,*,#2129,.F.);
#2797=ORIENTED_EDGE('',*,*,#2120,.T.);
#2798=ORIENTED_EDGE('',*,*,#2130,.F.);
#2799=ORIENTED_EDGE('',*,*,#2131,.T.);
#2800=ORIENTED_EDGE('',*,*,#2132,.T.);
#2801=ORIENTED_EDGE('',*,*,#2125,.T.);
#2802=ORIENTED_EDGE('',*,*,#2133,.F.);
#2803=ORIENTED_EDGE('',*,*,#2134,.F.);
#2804=ORIENTED_EDGE('',*,*,#2135,.T.);
#2805=ORIENTED_EDGE('',*,*,#2136,.T.);
#2806=ORIENTED_EDGE('',*,*,#2116,.T.);
#2807=ORIENTED_EDGE('',*,*,#2137,.F.);
#2808=ORIENTED_EDGE('',*,*,#2138,.F.);
#2809=ORIENTED_EDGE('',*,*,#2139,.T.);
#2810=ORIENTED_EDGE('',*,*,#2140,.F.);
#2811=ORIENTED_EDGE('',*,*,#2141,.F.);
#2812=ORIENTED_EDGE('',*,*,#2117,.T.);
#2813=ORIENTED_EDGE('',*,*,#2142,.F.);
#2814=ORIENTED_EDGE('',*,*,#2143,.T.);
#2815=ORIENTED_EDGE('',*,*,#2144,.F.);
#2816=ORIENTED_EDGE('',*,*,#2145,.F.);
#2817=ORIENTED_EDGE('',*,*,#2146,.T.);
#2818=ORIENTED_EDGE('',*,*,#2142,.T.);
#2819=ORIENTED_EDGE('',*,*,#2146,.F.);
#2820=ORIENTED_EDGE('',*,*,#2147,.F.);
#2821=ORIENTED_EDGE('',*,*,#2148,.F.);
#2822=ORIENTED_EDGE('',*,*,#2149,.F.);
#2823=ORIENTED_EDGE('',*,*,#2150,.F.);
#2824=ORIENTED_EDGE('',*,*,#2151,.F.);
#2825=ORIENTED_EDGE('',*,*,#2152,.F.);
#2826=ORIENTED_EDGE('',*,*,#2153,.F.);
#2827=ORIENTED_EDGE('',*,*,#2154,.F.);
#2828=ORIENTED_EDGE('',*,*,#2149,.T.);
#2829=ORIENTED_EDGE('',*,*,#2155,.F.);
#2830=ORIENTED_EDGE('',*,*,#2153,.T.);
#2831=ORIENTED_EDGE('',*,*,#2156,.T.);
#2832=ORIENTED_EDGE('',*,*,#2157,.F.);
#2833=ORIENTED_EDGE('',*,*,#2158,.F.);
#2834=ORIENTED_EDGE('',*,*,#2159,.T.);
#2835=ORIENTED_EDGE('',*,*,#2154,.T.);
#2836=ORIENTED_EDGE('',*,*,#2159,.F.);
#2837=ORIENTED_EDGE('',*,*,#2157,.T.);
#2838=ORIENTED_EDGE('',*,*,#2158,.T.);
#2839=ORIENTED_EDGE('',*,*,#2160,.T.);
#2840=ORIENTED_EDGE('',*,*,#2161,.F.);
#2841=ORIENTED_EDGE('',*,*,#2114,.F.);
#2842=ORIENTED_EDGE('',*,*,#2162,.F.);
#2843=ORIENTED_EDGE('',*,*,#2122,.F.);
#2844=ORIENTED_EDGE('',*,*,#2163,.F.);
#2845=ORIENTED_EDGE('',*,*,#2123,.F.);
#2846=ORIENTED_EDGE('',*,*,#2164,.F.);
#2847=ORIENTED_EDGE('',*,*,#2119,.F.);
#2848=ORIENTED_EDGE('',*,*,#2165,.F.);
#2849=ORIENTED_EDGE('',*,*,#2160,.F.);
#2850=ORIENTED_EDGE('',*,*,#2152,.T.);
#2851=ORIENTED_EDGE('',*,*,#2166,.T.);
#2852=ORIENTED_EDGE('',*,*,#2144,.T.);
#2853=ORIENTED_EDGE('',*,*,#2156,.F.);
#2854=ORIENTED_EDGE('',*,*,#2151,.T.);
#2855=ORIENTED_EDGE('',*,*,#2167,.T.);
#2856=ORIENTED_EDGE('',*,*,#2147,.T.);
#2857=ORIENTED_EDGE('',*,*,#2145,.T.);
#2858=ORIENTED_EDGE('',*,*,#2166,.F.);
#2859=ORIENTED_EDGE('',*,*,#2168,.F.);
#2860=ORIENTED_EDGE('',*,*,#2148,.T.);
#2861=ORIENTED_EDGE('',*,*,#2167,.F.);
#2862=ORIENTED_EDGE('',*,*,#2150,.T.);
#2863=ORIENTED_EDGE('',*,*,#2155,.T.);
#2864=ORIENTED_EDGE('',*,*,#2143,.F.);
#2865=ORIENTED_EDGE('',*,*,#2169,.T.);
#2866=ORIENTED_EDGE('',*,*,#2168,.T.);
#2867=ORIENTED_EDGE('',*,*,#2169,.F.);
#2868=ORIENTED_EDGE('',*,*,#2132,.F.);
#2869=ORIENTED_EDGE('',*,*,#2170,.T.);
#2870=ORIENTED_EDGE('',*,*,#2138,.T.);
#2871=ORIENTED_EDGE('',*,*,#2164,.T.);
#2872=ORIENTED_EDGE('',*,*,#2136,.F.);
#2873=ORIENTED_EDGE('',*,*,#2171,.T.);
#2874=ORIENTED_EDGE('',*,*,#2126,.T.);
#2875=ORIENTED_EDGE('',*,*,#2162,.T.);
#2876=ORIENTED_EDGE('',*,*,#2172,.T.);
#2877=ORIENTED_EDGE('',*,*,#2173,.T.);
#2878=ORIENTED_EDGE('',*,*,#2174,.T.);
#2879=ORIENTED_EDGE('',*,*,#2128,.T.);
#2880=ORIENTED_EDGE('',*,*,#2175,.T.);
#2881=ORIENTED_EDGE('',*,*,#2134,.T.);
#2882=ORIENTED_EDGE('',*,*,#2176,.T.);
#2883=ORIENTED_EDGE('',*,*,#2177,.T.);
#2884=ORIENTED_EDGE('',*,*,#2178,.T.);
#2885=ORIENTED_EDGE('',*,*,#2140,.T.);
#2886=ORIENTED_EDGE('',*,*,#2179,.T.);
#2887=ORIENTED_EDGE('',*,*,#2130,.T.);
#2888=ORIENTED_EDGE('',*,*,#2178,.F.);
#2889=ORIENTED_EDGE('',*,*,#2180,.T.);
#2890=ORIENTED_EDGE('',*,*,#2181,.T.);
#2891=ORIENTED_EDGE('',*,*,#2118,.T.);
#2892=ORIENTED_EDGE('',*,*,#2141,.T.);
#2893=ORIENTED_EDGE('',*,*,#2182,.F.);
#2894=ORIENTED_EDGE('',*,*,#2183,.T.);
#2895=ORIENTED_EDGE('',*,*,#2176,.F.);
#2896=ORIENTED_EDGE('',*,*,#2137,.T.);
#2897=ORIENTED_EDGE('',*,*,#2115,.T.);
#2898=ORIENTED_EDGE('',*,*,#2181,.F.);
#2899=ORIENTED_EDGE('',*,*,#2184,.T.);
#2900=ORIENTED_EDGE('',*,*,#2182,.T.);
#2901=ORIENTED_EDGE('',*,*,#2161,.T.);
#2902=ORIENTED_EDGE('',*,*,#2165,.T.);
#2903=ORIENTED_EDGE('',*,*,#2174,.F.);
#2904=ORIENTED_EDGE('',*,*,#2185,.T.);
#2905=ORIENTED_EDGE('',*,*,#2186,.T.);
#2906=ORIENTED_EDGE('',*,*,#2121,.T.);
#2907=ORIENTED_EDGE('',*,*,#2129,.T.);
#2908=ORIENTED_EDGE('',*,*,#2187,.F.);
#2909=ORIENTED_EDGE('',*,*,#2188,.T.);
#2910=ORIENTED_EDGE('',*,*,#2172,.F.);
#2911=ORIENTED_EDGE('',*,*,#2133,.T.);
#2912=ORIENTED_EDGE('',*,*,#2124,.T.);
#2913=ORIENTED_EDGE('',*,*,#2186,.F.);
#2914=ORIENTED_EDGE('',*,*,#2189,.T.);
#2915=ORIENTED_EDGE('',*,*,#2187,.T.);
#2916=ORIENTED_EDGE('',*,*,#2163,.T.);
#2917=ORIENTED_EDGE('',*,*,#2188,.F.);
#2918=ORIENTED_EDGE('',*,*,#2189,.F.);
#2919=ORIENTED_EDGE('',*,*,#2185,.F.);
#2920=ORIENTED_EDGE('',*,*,#2173,.F.);
#2921=ORIENTED_EDGE('',*,*,#2139,.F.);
#2922=ORIENTED_EDGE('',*,*,#2170,.F.);
#2923=ORIENTED_EDGE('',*,*,#2131,.F.);
#2924=ORIENTED_EDGE('',*,*,#2179,.F.);
#2925=ORIENTED_EDGE('',*,*,#2183,.F.);
#2926=ORIENTED_EDGE('',*,*,#2184,.F.);
#2927=ORIENTED_EDGE('',*,*,#2180,.F.);
#2928=ORIENTED_EDGE('',*,*,#2177,.F.);
#2929=ORIENTED_EDGE('',*,*,#2127,.F.);
#2930=ORIENTED_EDGE('',*,*,#2171,.F.);
#2931=ORIENTED_EDGE('',*,*,#2135,.F.);
#2932=ORIENTED_EDGE('',*,*,#2175,.F.);
#2933=ORIENTED_EDGE('',*,*,#2190,.F.);
#2934=ORIENTED_EDGE('',*,*,#2191,.T.);
#2935=ORIENTED_EDGE('',*,*,#2192,.T.);
#2936=ORIENTED_EDGE('',*,*,#2193,.F.);
#2937=ORIENTED_EDGE('',*,*,#2194,.T.);
#2938=ORIENTED_EDGE('',*,*,#2195,.T.);
#2939=ORIENTED_EDGE('',*,*,#2196,.F.);
#2940=ORIENTED_EDGE('',*,*,#2197,.T.);
#2941=ORIENTED_EDGE('',*,*,#2198,.T.);
#2942=ORIENTED_EDGE('',*,*,#2199,.T.);
#2943=ORIENTED_EDGE('',*,*,#2200,.F.);
#2944=ORIENTED_EDGE('',*,*,#2201,.F.);
#2945=ORIENTED_EDGE('',*,*,#2202,.F.);
#2946=ORIENTED_EDGE('',*,*,#2203,.F.);
#2947=ORIENTED_EDGE('',*,*,#2204,.F.);
#2948=ORIENTED_EDGE('',*,*,#2205,.F.);
#2949=ORIENTED_EDGE('',*,*,#2206,.T.);
#2950=ORIENTED_EDGE('',*,*,#2200,.T.);
#2951=ORIENTED_EDGE('',*,*,#2206,.F.);
#2952=ORIENTED_EDGE('',*,*,#2205,.T.);
#2953=ORIENTED_EDGE('',*,*,#2207,.F.);
#2954=ORIENTED_EDGE('',*,*,#2208,.T.);
#2955=ORIENTED_EDGE('',*,*,#2209,.T.);
#2956=ORIENTED_EDGE('',*,*,#2207,.T.);
#2957=ORIENTED_EDGE('',*,*,#2209,.F.);
#2958=ORIENTED_EDGE('',*,*,#2210,.F.);
#2959=ORIENTED_EDGE('',*,*,#2211,.F.);
#2960=ORIENTED_EDGE('',*,*,#2212,.F.);
#2961=ORIENTED_EDGE('',*,*,#2213,.F.);
#2962=ORIENTED_EDGE('',*,*,#2210,.T.);
#2963=ORIENTED_EDGE('',*,*,#2214,.T.);
#2964=ORIENTED_EDGE('',*,*,#2213,.T.);
#2965=ORIENTED_EDGE('',*,*,#2212,.T.);
#2966=ORIENTED_EDGE('',*,*,#2214,.F.);
#2967=ORIENTED_EDGE('',*,*,#2211,.T.);
#2968=ORIENTED_EDGE('',*,*,#2199,.F.);
#2969=ORIENTED_EDGE('',*,*,#2215,.T.);
#2970=ORIENTED_EDGE('',*,*,#2208,.F.);
#2971=ORIENTED_EDGE('',*,*,#2215,.F.);
#2972=ORIENTED_EDGE('',*,*,#2201,.T.);
#2973=ORIENTED_EDGE('',*,*,#2216,.F.);
#2974=ORIENTED_EDGE('',*,*,#2191,.F.);
#2975=ORIENTED_EDGE('',*,*,#2217,.F.);
#2976=ORIENTED_EDGE('',*,*,#2218,.T.);
#2977=ORIENTED_EDGE('',*,*,#2204,.T.);
#2978=ORIENTED_EDGE('',*,*,#2219,.F.);
#2979=ORIENTED_EDGE('',*,*,#2194,.F.);
#2980=ORIENTED_EDGE('',*,*,#2192,.F.);
#2981=ORIENTED_EDGE('',*,*,#2216,.T.);
#2982=ORIENTED_EDGE('',*,*,#2203,.T.);
#2983=ORIENTED_EDGE('',*,*,#2220,.F.);
#2984=ORIENTED_EDGE('',*,*,#2197,.F.);
#2985=ORIENTED_EDGE('',*,*,#2195,.F.);
#2986=ORIENTED_EDGE('',*,*,#2219,.T.);
#2987=ORIENTED_EDGE('',*,*,#2202,.T.);
#2988=ORIENTED_EDGE('',*,*,#2218,.F.);
#2989=ORIENTED_EDGE('',*,*,#2221,.F.);
#2990=ORIENTED_EDGE('',*,*,#2198,.F.);
#2991=ORIENTED_EDGE('',*,*,#2220,.T.);
#2992=ORIENTED_EDGE('',*,*,#2222,.F.);
#2993=ORIENTED_EDGE('',*,*,#2221,.T.);
#2994=ORIENTED_EDGE('',*,*,#2217,.T.);
#2995=ORIENTED_EDGE('',*,*,#2190,.T.);
#2996=ORIENTED_EDGE('',*,*,#2193,.T.);
#2997=ORIENTED_EDGE('',*,*,#2196,.T.);
#2998=ORIENTED_EDGE('',*,*,#2222,.T.);
#2999=ORIENTED_EDGE('',*,*,#2223,.T.);
#3000=ORIENTED_EDGE('',*,*,#2224,.F.);
#3001=ORIENTED_EDGE('',*,*,#2223,.F.);
#3002=ORIENTED_EDGE('',*,*,#2224,.T.);
#3003=ORIENTED_EDGE('',*,*,#2225,.T.);
#3004=ORIENTED_EDGE('',*,*,#2226,.F.);
#3005=ORIENTED_EDGE('',*,*,#2227,.F.);
#3006=ORIENTED_EDGE('',*,*,#2228,.T.);
#3007=ORIENTED_EDGE('',*,*,#2227,.T.);
#3008=ORIENTED_EDGE('',*,*,#2229,.T.);
#3009=ORIENTED_EDGE('',*,*,#2230,.T.);
#3010=ORIENTED_EDGE('',*,*,#2231,.T.);
#3011=ORIENTED_EDGE('',*,*,#2232,.T.);
#3012=ORIENTED_EDGE('',*,*,#2233,.T.);
#3013=ORIENTED_EDGE('',*,*,#2225,.F.);
#3014=ORIENTED_EDGE('',*,*,#2233,.F.);
#3015=ORIENTED_EDGE('',*,*,#2234,.T.);
#3016=ORIENTED_EDGE('',*,*,#2229,.F.);
#3017=ORIENTED_EDGE('',*,*,#2235,.T.);
#3018=ORIENTED_EDGE('',*,*,#2236,.T.);
#3019=ORIENTED_EDGE('',*,*,#2226,.T.);
#3020=ORIENTED_EDGE('',*,*,#2237,.T.);
#3021=ORIENTED_EDGE('',*,*,#2238,.F.);
#3022=ORIENTED_EDGE('',*,*,#2239,.F.);
#3023=ORIENTED_EDGE('',*,*,#2240,.F.);
#3024=ORIENTED_EDGE('',*,*,#2241,.T.);
#3025=ORIENTED_EDGE('',*,*,#2228,.F.);
#3026=ORIENTED_EDGE('',*,*,#2241,.F.);
#3027=ORIENTED_EDGE('',*,*,#2242,.F.);
#3028=ORIENTED_EDGE('',*,*,#2237,.F.);
#3029=ORIENTED_EDGE('',*,*,#2243,.F.);
#3030=ORIENTED_EDGE('',*,*,#2244,.F.);
#3031=ORIENTED_EDGE('',*,*,#2239,.T.);
#3032=ORIENTED_EDGE('',*,*,#2245,.T.);
#3033=ORIENTED_EDGE('',*,*,#2231,.F.);
#3034=ORIENTED_EDGE('',*,*,#2230,.F.);
#3035=ORIENTED_EDGE('',*,*,#2234,.F.);
#3036=ORIENTED_EDGE('',*,*,#2232,.F.);
#3037=ORIENTED_EDGE('',*,*,#2245,.F.);
#3038=ORIENTED_EDGE('',*,*,#2238,.T.);
#3039=ORIENTED_EDGE('',*,*,#2242,.T.);
#3040=ORIENTED_EDGE('',*,*,#2240,.T.);
#3041=ORIENTED_EDGE('',*,*,#2235,.F.);
#3042=ORIENTED_EDGE('',*,*,#2236,.F.);
#3043=ORIENTED_EDGE('',*,*,#2246,.T.);
#3044=ORIENTED_EDGE('',*,*,#2244,.T.);
#3045=ORIENTED_EDGE('',*,*,#2243,.T.);
#3046=ORIENTED_EDGE('',*,*,#2246,.F.);
#3047=ORIENTED_EDGE('',*,*,#2247,.T.);
#3048=ORIENTED_EDGE('',*,*,#2248,.T.);
#3049=ORIENTED_EDGE('',*,*,#2249,.F.);
#3050=ORIENTED_EDGE('',*,*,#2248,.F.);
#3051=ORIENTED_EDGE('',*,*,#2247,.F.);
#3052=ORIENTED_EDGE('',*,*,#2249,.T.);
#3053=ORIENTED_EDGE('',*,*,#2250,.F.);
#3054=ORIENTED_EDGE('',*,*,#2251,.T.);
#3055=ORIENTED_EDGE('',*,*,#2251,.F.);
#3056=ORIENTED_EDGE('',*,*,#2252,.T.);
#3057=ORIENTED_EDGE('',*,*,#2253,.T.);
#3058=ORIENTED_EDGE('',*,*,#2254,.T.);
#3059=ORIENTED_EDGE('',*,*,#2252,.F.);
#3060=ORIENTED_EDGE('',*,*,#2255,.T.);
#3061=ORIENTED_EDGE('',*,*,#2256,.T.);
#3062=ORIENTED_EDGE('',*,*,#2257,.T.);
#3063=ORIENTED_EDGE('',*,*,#2253,.F.);
#3064=ORIENTED_EDGE('',*,*,#2254,.F.);
#3065=ORIENTED_EDGE('',*,*,#2257,.F.);
#3066=ORIENTED_EDGE('',*,*,#2255,.F.);
#3067=ORIENTED_EDGE('',*,*,#2256,.F.);
#3068=ORIENTED_EDGE('',*,*,#2258,.T.);
#3069=ORIENTED_EDGE('',*,*,#2259,.T.);
#3070=ORIENTED_EDGE('',*,*,#2258,.F.);
#3071=ORIENTED_EDGE('',*,*,#2260,.T.);
#3072=ORIENTED_EDGE('',*,*,#2259,.F.);
#3073=ORIENTED_EDGE('',*,*,#2261,.T.);
#3074=ORIENTED_EDGE('',*,*,#2262,.T.);
#3075=ORIENTED_EDGE('',*,*,#2260,.F.);
#3076=ORIENTED_EDGE('',*,*,#2262,.F.);
#3077=ORIENTED_EDGE('',*,*,#2263,.T.);
#3078=ORIENTED_EDGE('',*,*,#2261,.F.);
#3079=ORIENTED_EDGE('',*,*,#2263,.F.);
#3080=ORIENTED_EDGE('',*,*,#2264,.T.);
#3081=ORIENTED_EDGE('',*,*,#2265,.T.);
#3082=ORIENTED_EDGE('',*,*,#2264,.F.);
#3083=ORIENTED_EDGE('',*,*,#2266,.T.);
#3084=ORIENTED_EDGE('',*,*,#2265,.F.);
#3085=ORIENTED_EDGE('',*,*,#2267,.F.);
#3086=ORIENTED_EDGE('',*,*,#2268,.F.);
#3087=ORIENTED_EDGE('',*,*,#2269,.F.);
#3088=ORIENTED_EDGE('',*,*,#2270,.F.);
#3089=ORIENTED_EDGE('',*,*,#2266,.F.);
#3090=ORIENTED_EDGE('',*,*,#2271,.T.);
#3091=ORIENTED_EDGE('',*,*,#2272,.T.);
#3092=ORIENTED_EDGE('',*,*,#2271,.F.);
#3093=ORIENTED_EDGE('',*,*,#2272,.F.);
#3094=ORIENTED_EDGE('',*,*,#2273,.F.);
#3095=ORIENTED_EDGE('',*,*,#2274,.F.);
#3096=ORIENTED_EDGE('',*,*,#2275,.F.);
#3097=ORIENTED_EDGE('',*,*,#2276,.F.);
#3098=ORIENTED_EDGE('',*,*,#2277,.T.);
#3099=ORIENTED_EDGE('',*,*,#2277,.F.);
#3100=ORIENTED_EDGE('',*,*,#2278,.T.);
#3101=ORIENTED_EDGE('',*,*,#2250,.T.);
#3102=ORIENTED_EDGE('',*,*,#2278,.F.);
#3103=ORIENTED_EDGE('',*,*,#2270,.T.);
#3104=ORIENTED_EDGE('',*,*,#2279,.T.);
#3105=ORIENTED_EDGE('',*,*,#2276,.T.);
#3106=ORIENTED_EDGE('',*,*,#2279,.F.);
#3107=ORIENTED_EDGE('',*,*,#2269,.T.);
#3108=ORIENTED_EDGE('',*,*,#2280,.T.);
#3109=ORIENTED_EDGE('',*,*,#2275,.T.);
#3110=ORIENTED_EDGE('',*,*,#2280,.F.);
#3111=ORIENTED_EDGE('',*,*,#2268,.T.);
#3112=ORIENTED_EDGE('',*,*,#2281,.T.);
#3113=ORIENTED_EDGE('',*,*,#2274,.T.);
#3114=ORIENTED_EDGE('',*,*,#2281,.F.);
#3115=ORIENTED_EDGE('',*,*,#2267,.T.);
#3116=ORIENTED_EDGE('',*,*,#2282,.T.);
#3117=ORIENTED_EDGE('',*,*,#2273,.T.);
#3118=ORIENTED_EDGE('',*,*,#2282,.F.);
#3119=ORIENTED_EDGE('',*,*,#2283,.F.);
#3120=ORIENTED_EDGE('',*,*,#2284,.T.);
#3121=ORIENTED_EDGE('',*,*,#2285,.T.);
#3122=ORIENTED_EDGE('',*,*,#2284,.F.);
#3123=ORIENTED_EDGE('',*,*,#2286,.F.);
#3124=ORIENTED_EDGE('',*,*,#2283,.T.);
#3125=ORIENTED_EDGE('',*,*,#2287,.F.);
#3126=ORIENTED_EDGE('',*,*,#2288,.T.);
#3127=ORIENTED_EDGE('',*,*,#2286,.T.);
#3128=ORIENTED_EDGE('',*,*,#2288,.F.);
#3129=ORIENTED_EDGE('',*,*,#2287,.T.);
#3130=ORIENTED_EDGE('',*,*,#2289,.F.);
#3131=ORIENTED_EDGE('',*,*,#2290,.F.);
#3132=ORIENTED_EDGE('',*,*,#2291,.T.);
#3133=ORIENTED_EDGE('',*,*,#2289,.T.);
#3134=ORIENTED_EDGE('',*,*,#2291,.F.);
#3135=ORIENTED_EDGE('',*,*,#2285,.F.);
#3136=ORIENTED_EDGE('',*,*,#2292,.T.);
#3137=ORIENTED_EDGE('',*,*,#2290,.T.);
#3138=ORIENTED_EDGE('',*,*,#2292,.F.);
#3139=ORIENTED_EDGE('',*,*,#2293,.F.);
#3140=ORIENTED_EDGE('',*,*,#2294,.T.);
#3141=ORIENTED_EDGE('',*,*,#2295,.T.);
#3142=ORIENTED_EDGE('',*,*,#2296,.T.);
#3143=ORIENTED_EDGE('',*,*,#2297,.T.);
#3144=ORIENTED_EDGE('',*,*,#2298,.F.);
#3145=ORIENTED_EDGE('',*,*,#2299,.T.);
#3146=ORIENTED_EDGE('',*,*,#2300,.T.);
#3147=ORIENTED_EDGE('',*,*,#2293,.T.);
#3148=ORIENTED_EDGE('',*,*,#2301,.T.);
#3149=ORIENTED_EDGE('',*,*,#2302,.T.);
#3150=ORIENTED_EDGE('',*,*,#2303,.T.);
#3151=ORIENTED_EDGE('',*,*,#2298,.T.);
#3152=ORIENTED_EDGE('',*,*,#2304,.T.);
#3153=ORIENTED_EDGE('',*,*,#2305,.F.);
#3154=ORIENTED_EDGE('',*,*,#2306,.F.);
#3155=ORIENTED_EDGE('',*,*,#2307,.T.);
#3156=ORIENTED_EDGE('',*,*,#2308,.T.);
#3157=ORIENTED_EDGE('',*,*,#2305,.T.);
#3158=ORIENTED_EDGE('',*,*,#2309,.T.);
#3159=ORIENTED_EDGE('',*,*,#2310,.F.);
#3160=ORIENTED_EDGE('',*,*,#2311,.T.);
#3161=ORIENTED_EDGE('',*,*,#2312,.T.);
#3162=ORIENTED_EDGE('',*,*,#2306,.T.);
#3163=ORIENTED_EDGE('',*,*,#2313,.T.);
#3164=ORIENTED_EDGE('',*,*,#2314,.T.);
#3165=ORIENTED_EDGE('',*,*,#2315,.T.);
#3166=ORIENTED_EDGE('',*,*,#2310,.T.);
#3167=ORIENTED_EDGE('',*,*,#2316,.T.);
#3168=ORIENTED_EDGE('',*,*,#2296,.F.);
#3169=ORIENTED_EDGE('',*,*,#2297,.F.);
#3170=ORIENTED_EDGE('',*,*,#2316,.F.);
#3171=ORIENTED_EDGE('',*,*,#2313,.F.);
#3172=ORIENTED_EDGE('',*,*,#2309,.F.);
#3173=ORIENTED_EDGE('',*,*,#2304,.F.);
#3174=ORIENTED_EDGE('',*,*,#2301,.F.);
#3175=ORIENTED_EDGE('',*,*,#2317,.F.);
#3176=ORIENTED_EDGE('',*,*,#2318,.F.);
#3177=ORIENTED_EDGE('',*,*,#2319,.T.);
#3178=ORIENTED_EDGE('',*,*,#2317,.T.);
#3179=ORIENTED_EDGE('',*,*,#2319,.F.);
#3180=ORIENTED_EDGE('',*,*,#2318,.T.);
#3181=ORIENTED_EDGE('',*,*,#2320,.F.);
#3182=ORIENTED_EDGE('',*,*,#2321,.T.);
#3183=ORIENTED_EDGE('',*,*,#2314,.F.);
#3184=ORIENTED_EDGE('',*,*,#2295,.F.);
#3185=ORIENTED_EDGE('',*,*,#2322,.T.);
#3186=ORIENTED_EDGE('',*,*,#2294,.F.);
#3187=ORIENTED_EDGE('',*,*,#2300,.F.);
#3188=ORIENTED_EDGE('',*,*,#2323,.T.);
#3189=ORIENTED_EDGE('',*,*,#2299,.F.);
#3190=ORIENTED_EDGE('',*,*,#2303,.F.);
#3191=ORIENTED_EDGE('',*,*,#2308,.F.);
#3192=ORIENTED_EDGE('',*,*,#2324,.T.);
#3193=ORIENTED_EDGE('',*,*,#2302,.F.);
#3194=ORIENTED_EDGE('',*,*,#2312,.F.);
#3195=ORIENTED_EDGE('',*,*,#2325,.T.);
#3196=ORIENTED_EDGE('',*,*,#2307,.F.);
#3197=ORIENTED_EDGE('',*,*,#2315,.F.);
#3198=ORIENTED_EDGE('',*,*,#2326,.T.);
#3199=ORIENTED_EDGE('',*,*,#2311,.F.);
#3200=ORIENTED_EDGE('',*,*,#2327,.F.);
#3201=ORIENTED_EDGE('',*,*,#2328,.F.);
#3202=ORIENTED_EDGE('',*,*,#2323,.F.);
#3203=ORIENTED_EDGE('',*,*,#2324,.F.);
#3204=ORIENTED_EDGE('',*,*,#2325,.F.);
#3205=ORIENTED_EDGE('',*,*,#2326,.F.);
#3206=ORIENTED_EDGE('',*,*,#2329,.T.);
#3207=ORIENTED_EDGE('',*,*,#2327,.T.);
#3208=ORIENTED_EDGE('',*,*,#2329,.F.);
#3209=ORIENTED_EDGE('',*,*,#2321,.F.);
#3210=ORIENTED_EDGE('',*,*,#2322,.F.);
#3211=ORIENTED_EDGE('',*,*,#2330,.F.);
#3212=ORIENTED_EDGE('',*,*,#2331,.T.);
#3213=ORIENTED_EDGE('',*,*,#2320,.T.);
#3214=ORIENTED_EDGE('',*,*,#2331,.F.);
#3215=ORIENTED_EDGE('',*,*,#2330,.T.);
#3216=ORIENTED_EDGE('',*,*,#2332,.F.);
#3217=ORIENTED_EDGE('',*,*,#2332,.T.);
#3218=ORIENTED_EDGE('',*,*,#2333,.T.);
#3219=ORIENTED_EDGE('',*,*,#2328,.T.);
#3220=ORIENTED_EDGE('',*,*,#2333,.F.);
#3221=ORIENTED_EDGE('',*,*,#2334,.T.);
#3222=ORIENTED_EDGE('',*,*,#2335,.T.);
#3223=ORIENTED_EDGE('',*,*,#2336,.T.);
#3224=ORIENTED_EDGE('',*,*,#2337,.T.);
#3225=ORIENTED_EDGE('',*,*,#2338,.T.);
#3226=ORIENTED_EDGE('',*,*,#2339,.T.);
#3227=ORIENTED_EDGE('',*,*,#2340,.F.);
#3228=ORIENTED_EDGE('',*,*,#2341,.T.);
#3229=ORIENTED_EDGE('',*,*,#2342,.F.);
#3230=ORIENTED_EDGE('',*,*,#2343,.T.);
#3231=ORIENTED_EDGE('',*,*,#2344,.F.);
#3232=ORIENTED_EDGE('',*,*,#2345,.T.);
#3233=ORIENTED_EDGE('',*,*,#2340,.T.);
#3234=ORIENTED_EDGE('',*,*,#2346,.T.);
#3235=ORIENTED_EDGE('',*,*,#2336,.F.);
#3236=ORIENTED_EDGE('',*,*,#2347,.T.);
#3237=ORIENTED_EDGE('',*,*,#2348,.T.);
#3238=ORIENTED_EDGE('',*,*,#2349,.T.);
#3239=ORIENTED_EDGE('',*,*,#2350,.F.);
#3240=ORIENTED_EDGE('',*,*,#2351,.T.);
#3241=ORIENTED_EDGE('',*,*,#2352,.T.);
#3242=ORIENTED_EDGE('',*,*,#2353,.T.);
#3243=ORIENTED_EDGE('',*,*,#2354,.T.);
#3244=ORIENTED_EDGE('',*,*,#2355,.T.);
#3245=ORIENTED_EDGE('',*,*,#2356,.T.);
#3246=ORIENTED_EDGE('',*,*,#2357,.F.);
#3247=ORIENTED_EDGE('',*,*,#2358,.T.);
#3248=ORIENTED_EDGE('',*,*,#2359,.T.);
#3249=ORIENTED_EDGE('',*,*,#2360,.T.);
#3250=ORIENTED_EDGE('',*,*,#2361,.T.);
#3251=ORIENTED_EDGE('',*,*,#2362,.T.);
#3252=ORIENTED_EDGE('',*,*,#2363,.T.);
#3253=ORIENTED_EDGE('',*,*,#2364,.T.);
#3254=ORIENTED_EDGE('',*,*,#2365,.F.);
#3255=ORIENTED_EDGE('',*,*,#2366,.T.);
#3256=ORIENTED_EDGE('',*,*,#2367,.T.);
#3257=ORIENTED_EDGE('',*,*,#2368,.T.);
#3258=ORIENTED_EDGE('',*,*,#2369,.T.);
#3259=ORIENTED_EDGE('',*,*,#2334,.F.);
#3260=ORIENTED_EDGE('',*,*,#2370,.T.);
#3261=ORIENTED_EDGE('',*,*,#2342,.T.);
#3262=ORIENTED_EDGE('',*,*,#2371,.T.);
#3263=ORIENTED_EDGE('',*,*,#2372,.T.);
#3264=ORIENTED_EDGE('',*,*,#2373,.T.);
#3265=ORIENTED_EDGE('',*,*,#2374,.F.);
#3266=ORIENTED_EDGE('',*,*,#2375,.T.);
#3267=ORIENTED_EDGE('',*,*,#2376,.T.);
#3268=ORIENTED_EDGE('',*,*,#2377,.T.);
#3269=ORIENTED_EDGE('',*,*,#2378,.T.);
#3270=ORIENTED_EDGE('',*,*,#2379,.T.);
#3271=ORIENTED_EDGE('',*,*,#2357,.T.);
#3272=ORIENTED_EDGE('',*,*,#2380,.T.);
#3273=ORIENTED_EDGE('',*,*,#2381,.T.);
#3274=ORIENTED_EDGE('',*,*,#2382,.T.);
#3275=ORIENTED_EDGE('',*,*,#2383,.T.);
#3276=ORIENTED_EDGE('',*,*,#2384,.T.);
#3277=ORIENTED_EDGE('',*,*,#2385,.F.);
#3278=ORIENTED_EDGE('',*,*,#2386,.T.);
#3279=ORIENTED_EDGE('',*,*,#2359,.F.);
#3280=ORIENTED_EDGE('',*,*,#2387,.T.);
#3281=ORIENTED_EDGE('',*,*,#2388,.F.);
#3282=ORIENTED_EDGE('',*,*,#2389,.T.);
#3283=ORIENTED_EDGE('',*,*,#2350,.T.);
#3284=ORIENTED_EDGE('',*,*,#2390,.T.);
#3285=ORIENTED_EDGE('',*,*,#2365,.T.);
#3286=ORIENTED_EDGE('',*,*,#2391,.T.);
#3287=ORIENTED_EDGE('',*,*,#2392,.T.);
#3288=ORIENTED_EDGE('',*,*,#2393,.T.);
#3289=ORIENTED_EDGE('',*,*,#2363,.F.);
#3290=ORIENTED_EDGE('',*,*,#2394,.T.);
#3291=ORIENTED_EDGE('',*,*,#2352,.F.);
#3292=ORIENTED_EDGE('',*,*,#2395,.T.);
#3293=ORIENTED_EDGE('',*,*,#2396,.F.);
#3294=ORIENTED_EDGE('',*,*,#2397,.T.);
#3295=ORIENTED_EDGE('',*,*,#2374,.T.);
#3296=ORIENTED_EDGE('',*,*,#2398,.T.);
#3297=ORIENTED_EDGE('',*,*,#2399,.T.);
#3298=ORIENTED_EDGE('',*,*,#2400,.T.);
#3299=ORIENTED_EDGE('',*,*,#2401,.T.);
#3300=ORIENTED_EDGE('',*,*,#2402,.T.);
#3301=ORIENTED_EDGE('',*,*,#2403,.F.);
#3302=ORIENTED_EDGE('',*,*,#2404,.T.);
#3303=ORIENTED_EDGE('',*,*,#2376,.F.);
#3304=ORIENTED_EDGE('',*,*,#2405,.T.);
#3305=ORIENTED_EDGE('',*,*,#2406,.F.);
#3306=ORIENTED_EDGE('',*,*,#2407,.T.);
#3307=ORIENTED_EDGE('',*,*,#2408,.F.);
#3308=ORIENTED_EDGE('',*,*,#2367,.F.);
#3309=ORIENTED_EDGE('',*,*,#2409,.T.);
#3310=ORIENTED_EDGE('',*,*,#2410,.T.);
#3311=ORIENTED_EDGE('',*,*,#2411,.T.);
#3312=ORIENTED_EDGE('',*,*,#2412,.F.);
#3313=ORIENTED_EDGE('',*,*,#2413,.T.);
#3314=ORIENTED_EDGE('',*,*,#2414,.T.);
#3315=ORIENTED_EDGE('',*,*,#2415,.T.);
#3316=ORIENTED_EDGE('',*,*,#2378,.F.);
#3317=ORIENTED_EDGE('',*,*,#2416,.T.);
#3318=ORIENTED_EDGE('',*,*,#2417,.T.);
#3319=ORIENTED_EDGE('',*,*,#2418,.T.);
#3320=ORIENTED_EDGE('',*,*,#2372,.F.);
#3321=ORIENTED_EDGE('',*,*,#2419,.T.);
#3322=ORIENTED_EDGE('',*,*,#2420,.T.);
#3323=ORIENTED_EDGE('',*,*,#2421,.T.);
#3324=ORIENTED_EDGE('',*,*,#2368,.F.);
#3325=ORIENTED_EDGE('',*,*,#2408,.T.);
#3326=ORIENTED_EDGE('',*,*,#2354,.F.);
#3327=ORIENTED_EDGE('',*,*,#2422,.T.);
#3328=ORIENTED_EDGE('',*,*,#2420,.F.);
#3329=ORIENTED_EDGE('',*,*,#2423,.T.);
#3330=ORIENTED_EDGE('',*,*,#2348,.F.);
#3331=ORIENTED_EDGE('',*,*,#2424,.T.);
#3332=ORIENTED_EDGE('',*,*,#2417,.F.);
#3333=ORIENTED_EDGE('',*,*,#2425,.T.);
#3334=ORIENTED_EDGE('',*,*,#2426,.F.);
#3335=ORIENTED_EDGE('',*,*,#2427,.T.);
#3336=ORIENTED_EDGE('',*,*,#2414,.F.);
#3337=ORIENTED_EDGE('',*,*,#2428,.T.);
#3338=ORIENTED_EDGE('',*,*,#2361,.F.);
#3339=ORIENTED_EDGE('',*,*,#2429,.T.);
#3340=ORIENTED_EDGE('',*,*,#2410,.F.);
#3341=ORIENTED_EDGE('',*,*,#2430,.T.);
#3342=ORIENTED_EDGE('',*,*,#2355,.F.);
#3343=ORIENTED_EDGE('',*,*,#2403,.T.);
#3344=ORIENTED_EDGE('',*,*,#2431,.T.);
#3345=ORIENTED_EDGE('',*,*,#2399,.F.);
#3346=ORIENTED_EDGE('',*,*,#2432,.T.);
#3347=ORIENTED_EDGE('',*,*,#2426,.T.);
#3348=ORIENTED_EDGE('',*,*,#2433,.T.);
#3349=ORIENTED_EDGE('',*,*,#2385,.T.);
#3350=ORIENTED_EDGE('',*,*,#2434,.T.);
#3351=ORIENTED_EDGE('',*,*,#2381,.F.);
#3352=ORIENTED_EDGE('',*,*,#2435,.T.);
#3353=ORIENTED_EDGE('',*,*,#2412,.T.);
#3354=ORIENTED_EDGE('',*,*,#2436,.T.);
#3355=ORIENTED_EDGE('',*,*,#2437,.T.);
#3356=ORIENTED_EDGE('',*,*,#2438,.T.);
#3357=ORIENTED_EDGE('',*,*,#2439,.T.);
#3358=ORIENTED_EDGE('',*,*,#2396,.T.);
#3359=ORIENTED_EDGE('',*,*,#2440,.T.);
#3360=ORIENTED_EDGE('',*,*,#2441,.T.);
#3361=ORIENTED_EDGE('',*,*,#2442,.F.);
#3362=ORIENTED_EDGE('',*,*,#2441,.F.);
#3363=ORIENTED_EDGE('',*,*,#2443,.T.);
#3364=ORIENTED_EDGE('',*,*,#2392,.F.);
#3365=ORIENTED_EDGE('',*,*,#2444,.T.);
#3366=ORIENTED_EDGE('',*,*,#2438,.F.);
#3367=ORIENTED_EDGE('',*,*,#2445,.T.);
#3368=ORIENTED_EDGE('',*,*,#2383,.F.);
#3369=ORIENTED_EDGE('',*,*,#2446,.T.);
#3370=ORIENTED_EDGE('',*,*,#2388,.T.);
#3371=ORIENTED_EDGE('',*,*,#2447,.T.);
#3372=ORIENTED_EDGE('',*,*,#2406,.T.);
#3373=ORIENTED_EDGE('',*,*,#2448,.T.);
#3374=ORIENTED_EDGE('',*,*,#2401,.F.);
#3375=ORIENTED_EDGE('',*,*,#2449,.T.);
#3376=ORIENTED_EDGE('',*,*,#2338,.F.);
#3377=ORIENTED_EDGE('',*,*,#2450,.T.);
#3378=ORIENTED_EDGE('',*,*,#2344,.T.);
#3379=ORIENTED_EDGE('',*,*,#2442,.T.);
#3380=ORIENTED_EDGE('',*,*,#2451,.T.);
#3381=ORIENTED_EDGE('',*,*,#2452,.T.);
#3382=ORIENTED_EDGE('',*,*,#2453,.T.);
#3383=ORIENTED_EDGE('',*,*,#2454,.T.);
#3384=ORIENTED_EDGE('',*,*,#2437,.F.);
#3385=ORIENTED_EDGE('',*,*,#2455,.F.);
#3386=ORIENTED_EDGE('',*,*,#2456,.F.);
#3387=ORIENTED_EDGE('',*,*,#2457,.F.);
#3388=ORIENTED_EDGE('',*,*,#2458,.F.);
#3389=ORIENTED_EDGE('',*,*,#2456,.T.);
#3390=ORIENTED_EDGE('',*,*,#2459,.F.);
#3391=ORIENTED_EDGE('',*,*,#2451,.F.);
#3392=ORIENTED_EDGE('',*,*,#2460,.T.);
#3393=ORIENTED_EDGE('',*,*,#2457,.T.);
#3394=ORIENTED_EDGE('',*,*,#2460,.F.);
#3395=ORIENTED_EDGE('',*,*,#2454,.F.);
#3396=ORIENTED_EDGE('',*,*,#2461,.T.);
#3397=ORIENTED_EDGE('',*,*,#2458,.T.);
#3398=ORIENTED_EDGE('',*,*,#2461,.F.);
#3399=ORIENTED_EDGE('',*,*,#2453,.F.);
#3400=ORIENTED_EDGE('',*,*,#2462,.T.);
#3401=ORIENTED_EDGE('',*,*,#2455,.T.);
#3402=ORIENTED_EDGE('',*,*,#2462,.F.);
#3403=ORIENTED_EDGE('',*,*,#2452,.F.);
#3404=ORIENTED_EDGE('',*,*,#2459,.T.);
#3405=ORIENTED_EDGE('',*,*,#2395,.F.);
#3406=ORIENTED_EDGE('',*,*,#2351,.F.);
#3407=ORIENTED_EDGE('',*,*,#2393,.F.);
#3408=ORIENTED_EDGE('',*,*,#2443,.F.);
#3409=ORIENTED_EDGE('',*,*,#2440,.F.);
#3410=ORIENTED_EDGE('',*,*,#2343,.F.);
#3411=ORIENTED_EDGE('',*,*,#2370,.F.);
#3412=ORIENTED_EDGE('',*,*,#2339,.F.);
#3413=ORIENTED_EDGE('',*,*,#2449,.F.);
#3414=ORIENTED_EDGE('',*,*,#2391,.F.);
#3415=ORIENTED_EDGE('',*,*,#2364,.F.);
#3416=ORIENTED_EDGE('',*,*,#2397,.F.);
#3417=ORIENTED_EDGE('',*,*,#2439,.F.);
#3418=ORIENTED_EDGE('',*,*,#2444,.F.);
#3419=ORIENTED_EDGE('',*,*,#2337,.F.);
#3420=ORIENTED_EDGE('',*,*,#2346,.F.);
#3421=ORIENTED_EDGE('',*,*,#2345,.F.);
#3422=ORIENTED_EDGE('',*,*,#2450,.F.);
#3423=ORIENTED_EDGE('',*,*,#2400,.F.);
#3424=ORIENTED_EDGE('',*,*,#2431,.F.);
#3425=ORIENTED_EDGE('',*,*,#2407,.F.);
#3426=ORIENTED_EDGE('',*,*,#2447,.F.);
#3427=ORIENTED_EDGE('',*,*,#2387,.F.);
#3428=ORIENTED_EDGE('',*,*,#2358,.F.);
#3429=ORIENTED_EDGE('',*,*,#2384,.F.);
#3430=ORIENTED_EDGE('',*,*,#2445,.F.);
#3431=ORIENTED_EDGE('',*,*,#2382,.F.);
#3432=ORIENTED_EDGE('',*,*,#2434,.F.);
#3433=ORIENTED_EDGE('',*,*,#2389,.F.);
#3434=ORIENTED_EDGE('',*,*,#2446,.F.);
#3435=ORIENTED_EDGE('',*,*,#2405,.F.);
#3436=ORIENTED_EDGE('',*,*,#2375,.F.);
#3437=ORIENTED_EDGE('',*,*,#2402,.F.);
#3438=ORIENTED_EDGE('',*,*,#2448,.F.);
#3439=ORIENTED_EDGE('',*,*,#2347,.F.);
#3440=ORIENTED_EDGE('',*,*,#2335,.F.);
#3441=ORIENTED_EDGE('',*,*,#2373,.F.);
#3442=ORIENTED_EDGE('',*,*,#2418,.F.);
#3443=ORIENTED_EDGE('',*,*,#2424,.F.);
#3444=ORIENTED_EDGE('',*,*,#2349,.F.);
#3445=ORIENTED_EDGE('',*,*,#2423,.F.);
#3446=ORIENTED_EDGE('',*,*,#2419,.F.);
#3447=ORIENTED_EDGE('',*,*,#2371,.F.);
#3448=ORIENTED_EDGE('',*,*,#2341,.F.);
#3449=ORIENTED_EDGE('',*,*,#2432,.F.);
#3450=ORIENTED_EDGE('',*,*,#2398,.F.);
#3451=ORIENTED_EDGE('',*,*,#2379,.F.);
#3452=ORIENTED_EDGE('',*,*,#2415,.F.);
#3453=ORIENTED_EDGE('',*,*,#2427,.F.);
#3454=ORIENTED_EDGE('',*,*,#2433,.F.);
#3455=ORIENTED_EDGE('',*,*,#2425,.F.);
#3456=ORIENTED_EDGE('',*,*,#2416,.F.);
#3457=ORIENTED_EDGE('',*,*,#2377,.F.);
#3458=ORIENTED_EDGE('',*,*,#2404,.F.);
#3459=ORIENTED_EDGE('',*,*,#2369,.F.);
#3460=ORIENTED_EDGE('',*,*,#2421,.F.);
#3461=ORIENTED_EDGE('',*,*,#2422,.F.);
#3462=ORIENTED_EDGE('',*,*,#2353,.F.);
#3463=ORIENTED_EDGE('',*,*,#2394,.F.);
#3464=ORIENTED_EDGE('',*,*,#2366,.F.);
#3465=ORIENTED_EDGE('',*,*,#2390,.F.);
#3466=ORIENTED_EDGE('',*,*,#2356,.F.);
#3467=ORIENTED_EDGE('',*,*,#2430,.F.);
#3468=ORIENTED_EDGE('',*,*,#2409,.F.);
#3469=ORIENTED_EDGE('',*,*,#2436,.F.);
#3470=ORIENTED_EDGE('',*,*,#2411,.F.);
#3471=ORIENTED_EDGE('',*,*,#2429,.F.);
#3472=ORIENTED_EDGE('',*,*,#2360,.F.);
#3473=ORIENTED_EDGE('',*,*,#2386,.F.);
#3474=ORIENTED_EDGE('',*,*,#2435,.F.);
#3475=ORIENTED_EDGE('',*,*,#2380,.F.);
#3476=ORIENTED_EDGE('',*,*,#2362,.F.);
#3477=ORIENTED_EDGE('',*,*,#2428,.F.);
#3478=ORIENTED_EDGE('',*,*,#2413,.F.);
#3479=ORIENTED_EDGE('',*,*,#2463,.F.);
#3480=ORIENTED_EDGE('',*,*,#2464,.F.);
#3481=ORIENTED_EDGE('',*,*,#2465,.F.);
#3482=ORIENTED_EDGE('',*,*,#2466,.F.);
#3483=ORIENTED_EDGE('',*,*,#2467,.T.);
#3484=ORIENTED_EDGE('',*,*,#2468,.F.);
#3485=ORIENTED_EDGE('',*,*,#2469,.F.);
#3486=ORIENTED_EDGE('',*,*,#2470,.F.);
#3487=ORIENTED_EDGE('',*,*,#2471,.F.);
#3488=ORIENTED_EDGE('',*,*,#2472,.F.);
#3489=ORIENTED_EDGE('',*,*,#2464,.T.);
#3490=ORIENTED_EDGE('',*,*,#2473,.F.);
#3491=ORIENTED_EDGE('',*,*,#2474,.F.);
#3492=ORIENTED_EDGE('',*,*,#2475,.F.);
#3493=ORIENTED_EDGE('',*,*,#2476,.F.);
#3494=ORIENTED_EDGE('',*,*,#2477,.F.);
#3495=ORIENTED_EDGE('',*,*,#2470,.T.);
#3496=ORIENTED_EDGE('',*,*,#2478,.F.);
#3497=ORIENTED_EDGE('',*,*,#2479,.F.);
#3498=ORIENTED_EDGE('',*,*,#2480,.F.);
#3499=ORIENTED_EDGE('',*,*,#2481,.F.);
#3500=ORIENTED_EDGE('',*,*,#2482,.F.);
#3501=ORIENTED_EDGE('',*,*,#2475,.T.);
#3502=ORIENTED_EDGE('',*,*,#2483,.F.);
#3503=ORIENTED_EDGE('',*,*,#2484,.F.);
#3504=ORIENTED_EDGE('',*,*,#2485,.F.);
#3505=ORIENTED_EDGE('',*,*,#2486,.F.);
#3506=ORIENTED_EDGE('',*,*,#2487,.F.);
#3507=ORIENTED_EDGE('',*,*,#2480,.T.);
#3508=ORIENTED_EDGE('',*,*,#2488,.F.);
#3509=ORIENTED_EDGE('',*,*,#2489,.F.);
#3510=ORIENTED_EDGE('',*,*,#2467,.F.);
#3511=ORIENTED_EDGE('',*,*,#2490,.F.);
#3512=ORIENTED_EDGE('',*,*,#2491,.F.);
#3513=ORIENTED_EDGE('',*,*,#2485,.T.);
#3514=ORIENTED_EDGE('',*,*,#2492,.F.);
#3515=ORIENTED_EDGE('',*,*,#2493,.F.);
#3516=ORIENTED_EDGE('',*,*,#2494,.F.);
#3517=ORIENTED_EDGE('',*,*,#2495,.F.);
#3518=ORIENTED_EDGE('',*,*,#2496,.F.);
#3519=ORIENTED_EDGE('',*,*,#2497,.T.);
#3520=ORIENTED_EDGE('',*,*,#2498,.F.);
#3521=ORIENTED_EDGE('',*,*,#2499,.T.);
#3522=ORIENTED_EDGE('',*,*,#2500,.T.);
#3523=ORIENTED_EDGE('',*,*,#2501,.T.);
#3524=ORIENTED_EDGE('',*,*,#2502,.T.);
#3525=ORIENTED_EDGE('',*,*,#2503,.T.);
#3526=ORIENTED_EDGE('',*,*,#2504,.T.);
#3527=ORIENTED_EDGE('',*,*,#2505,.T.);
#3528=ORIENTED_EDGE('',*,*,#2506,.F.);
#3529=ORIENTED_EDGE('',*,*,#2506,.T.);
#3530=ORIENTED_EDGE('',*,*,#2507,.T.);
#3531=ORIENTED_EDGE('',*,*,#2499,.F.);
#3532=ORIENTED_EDGE('',*,*,#2507,.F.);
#3533=ORIENTED_EDGE('',*,*,#2466,.T.);
#3534=ORIENTED_EDGE('',*,*,#2501,.F.);
#3535=ORIENTED_EDGE('',*,*,#2490,.T.);
#3536=ORIENTED_EDGE('',*,*,#2486,.T.);
#3537=ORIENTED_EDGE('',*,*,#2491,.T.);
#3538=ORIENTED_EDGE('',*,*,#2500,.F.);
#3539=ORIENTED_EDGE('',*,*,#2481,.T.);
#3540=ORIENTED_EDGE('',*,*,#2487,.T.);
#3541=ORIENTED_EDGE('',*,*,#2505,.F.);
#3542=ORIENTED_EDGE('',*,*,#2476,.T.);
#3543=ORIENTED_EDGE('',*,*,#2482,.T.);
#3544=ORIENTED_EDGE('',*,*,#2504,.F.);
#3545=ORIENTED_EDGE('',*,*,#2471,.T.);
#3546=ORIENTED_EDGE('',*,*,#2477,.T.);
#3547=ORIENTED_EDGE('',*,*,#2503,.F.);
#3548=ORIENTED_EDGE('',*,*,#2465,.T.);
#3549=ORIENTED_EDGE('',*,*,#2472,.T.);
#3550=ORIENTED_EDGE('',*,*,#2502,.F.);
#3551=ORIENTED_EDGE('',*,*,#2484,.T.);
#3552=ORIENTED_EDGE('',*,*,#2494,.T.);
#3553=ORIENTED_EDGE('',*,*,#2492,.T.);
#3554=ORIENTED_EDGE('',*,*,#2479,.T.);
#3555=ORIENTED_EDGE('',*,*,#2495,.T.);
#3556=ORIENTED_EDGE('',*,*,#2488,.T.);
#3557=ORIENTED_EDGE('',*,*,#2474,.T.);
#3558=ORIENTED_EDGE('',*,*,#2496,.T.);
#3559=ORIENTED_EDGE('',*,*,#2483,.T.);
#3560=ORIENTED_EDGE('',*,*,#2478,.T.);
#3561=ORIENTED_EDGE('',*,*,#2469,.T.);
#3562=ORIENTED_EDGE('',*,*,#2497,.F.);
#3563=ORIENTED_EDGE('',*,*,#2473,.T.);
#3564=ORIENTED_EDGE('',*,*,#2463,.T.);
#3565=ORIENTED_EDGE('',*,*,#2498,.T.);
#3566=ORIENTED_EDGE('',*,*,#2468,.T.);
#3567=ORIENTED_EDGE('',*,*,#2489,.T.);
#3568=ORIENTED_EDGE('',*,*,#2493,.T.);
#3569=ORIENTED_EDGE('',*,*,#2508,.F.);
#3570=ORIENTED_EDGE('',*,*,#2509,.T.);
#3571=ORIENTED_EDGE('',*,*,#2510,.T.);
#3572=ORIENTED_EDGE('',*,*,#2511,.F.);
#3573=ORIENTED_EDGE('',*,*,#2512,.F.);
#3574=ORIENTED_EDGE('',*,*,#2513,.F.);
#3575=ORIENTED_EDGE('',*,*,#2511,.T.);
#3576=ORIENTED_EDGE('',*,*,#2514,.T.);
#3577=ORIENTED_EDGE('',*,*,#2515,.F.);
#3578=ORIENTED_EDGE('',*,*,#2516,.F.);
#3579=ORIENTED_EDGE('',*,*,#2517,.F.);
#3580=ORIENTED_EDGE('',*,*,#2515,.T.);
#3581=ORIENTED_EDGE('',*,*,#2518,.T.);
#3582=ORIENTED_EDGE('',*,*,#2519,.F.);
#3583=ORIENTED_EDGE('',*,*,#2520,.F.);
#3584=ORIENTED_EDGE('',*,*,#2521,.F.);
#3585=ORIENTED_EDGE('',*,*,#2519,.T.);
#3586=ORIENTED_EDGE('',*,*,#2522,.T.);
#3587=ORIENTED_EDGE('',*,*,#2523,.F.);
#3588=ORIENTED_EDGE('',*,*,#2524,.F.);
#3589=ORIENTED_EDGE('',*,*,#2525,.F.);
#3590=ORIENTED_EDGE('',*,*,#2523,.T.);
#3591=ORIENTED_EDGE('',*,*,#2526,.T.);
#3592=ORIENTED_EDGE('',*,*,#2527,.F.);
#3593=ORIENTED_EDGE('',*,*,#2528,.F.);
#3594=ORIENTED_EDGE('',*,*,#2529,.F.);
#3595=ORIENTED_EDGE('',*,*,#2527,.T.);
#3596=ORIENTED_EDGE('',*,*,#2530,.T.);
#3597=ORIENTED_EDGE('',*,*,#2509,.F.);
#3598=ORIENTED_EDGE('',*,*,#2531,.F.);
#3599=ORIENTED_EDGE('',*,*,#2532,.T.);
#3600=ORIENTED_EDGE('',*,*,#2533,.T.);
#3601=ORIENTED_EDGE('',*,*,#2534,.F.);
#3602=ORIENTED_EDGE('',*,*,#2533,.F.);
#3603=ORIENTED_EDGE('',*,*,#2532,.F.);
#3604=ORIENTED_EDGE('',*,*,#2510,.F.);
#3605=ORIENTED_EDGE('',*,*,#2530,.F.);
#3606=ORIENTED_EDGE('',*,*,#2526,.F.);
#3607=ORIENTED_EDGE('',*,*,#2522,.F.);
#3608=ORIENTED_EDGE('',*,*,#2518,.F.);
#3609=ORIENTED_EDGE('',*,*,#2514,.F.);
#3610=ORIENTED_EDGE('',*,*,#2534,.T.);
#3611=ORIENTED_EDGE('',*,*,#2528,.T.);
#3612=ORIENTED_EDGE('',*,*,#2529,.T.);
#3613=ORIENTED_EDGE('',*,*,#2535,.F.);
#3614=ORIENTED_EDGE('',*,*,#2524,.T.);
#3615=ORIENTED_EDGE('',*,*,#2525,.T.);
#3616=ORIENTED_EDGE('',*,*,#2536,.F.);
#3617=ORIENTED_EDGE('',*,*,#2520,.T.);
#3618=ORIENTED_EDGE('',*,*,#2521,.T.);
#3619=ORIENTED_EDGE('',*,*,#2537,.F.);
#3620=ORIENTED_EDGE('',*,*,#2516,.T.);
#3621=ORIENTED_EDGE('',*,*,#2517,.T.);
#3622=ORIENTED_EDGE('',*,*,#2538,.F.);
#3623=ORIENTED_EDGE('',*,*,#2512,.T.);
#3624=ORIENTED_EDGE('',*,*,#2513,.T.);
#3625=ORIENTED_EDGE('',*,*,#2539,.F.);
#3626=ORIENTED_EDGE('',*,*,#2508,.T.);
#3627=ORIENTED_EDGE('',*,*,#2540,.F.);
#3628=ORIENTED_EDGE('',*,*,#2531,.T.);
#3629=ORIENTED_EDGE('',*,*,#2535,.T.);
#3630=ORIENTED_EDGE('',*,*,#2540,.T.);
#3631=ORIENTED_EDGE('',*,*,#2539,.T.);
#3632=ORIENTED_EDGE('',*,*,#2538,.T.);
#3633=ORIENTED_EDGE('',*,*,#2537,.T.);
#3634=ORIENTED_EDGE('',*,*,#2536,.T.);
#3635=TOROIDAL_SURFACE('',#4016,88.0000000000002,2.);
#3636=TOROIDAL_SURFACE('',#4022,58.0000000000002,2.);
#3637=TOROIDAL_SURFACE('',#4065,41.9999999999999,2.);
#3638=TOROIDAL_SURFACE('',#4070,48.,8.);
#3639=TOROIDAL_SURFACE('',#4094,38.5,2.5);
#3640=TOROIDAL_SURFACE('',#4131,40.999999999998,1.);
#3641=TOROIDAL_SURFACE('',#4133,82.9999999999998,1.);
#3642=TOROIDAL_SURFACE('',#4212,7.,1.);
#3643=TOROIDAL_SURFACE('',#4305,34.6410161513776,5.35898384862241);
#3644=TOROIDAL_SURFACE('',#4307,34.6410161513776,5.35898384862241);
#3645=TOROIDAL_SURFACE('',#4309,34.6410161513776,5.35898384862241);
#3646=TOROIDAL_SURFACE('',#4311,34.6410161513776,5.35898384862241);
#3647=TOROIDAL_SURFACE('',#4313,34.6410161513776,5.35898384862241);
#3648=TOROIDAL_SURFACE('',#4315,34.6410161513776,5.35898384862241);
#3649=TOROIDAL_SURFACE('',#4355,79.,10.);
#3650=TOROIDAL_SURFACE('',#4386,18.,2.);
#3651=TOROIDAL_SURFACE('',#4387,18.,2.);
#3652=TOROIDAL_SURFACE('',#4388,18.,2.);
#3653=TOROIDAL_SURFACE('',#4389,18.,2.);
#3654=TOROIDAL_SURFACE('',#4390,18.,2.);
#3655=TOROIDAL_SURFACE('',#4391,18.,2.);
#3656=TOROIDAL_SURFACE('',#4392,18.,2.);
#3657=TOROIDAL_SURFACE('',#4393,18.,2.);
#3658=ADVANCED_FACE('',(#810),#3635,.T.);
#3659=ADVANCED_FACE('',(#811),#753,.T.);
#3660=ADVANCED_FACE('',(#812),#3636,.F.);
#3661=ADVANCED_FACE('',(#813,#195,#196,#197),#268,.T.);
#3662=ADVANCED_FACE('',(#814,#198),#269,.T.);
#3663=ADVANCED_FACE('',(#815),#163,.F.);
#3664=ADVANCED_FACE('',(#816),#754,.F.);
#3665=ADVANCED_FACE('',(#817,#199),#270,.T.);
#3666=ADVANCED_FACE('',(#818),#755,.F.);
#3667=ADVANCED_FACE('',(#819,#200,#201,#202,#203,#204),#271,.T.);
#3668=ADVANCED_FACE('',(#820),#756,.T.);
#3669=ADVANCED_FACE('',(#821,#205,#206,#207,#208,#209),#272,.T.);
#3670=ADVANCED_FACE('',(#822),#757,.T.);
#3671=ADVANCED_FACE('',(#823),#3637,.F.);
#3672=ADVANCED_FACE('',(#824,#210),#273,.T.);
#3673=ADVANCED_FACE('',(#825),#3638,.T.);
#3674=ADVANCED_FACE('',(#826),#758,.T.);
#3675=ADVANCED_FACE('',(#827),#759,.T.);
#3676=ADVANCED_FACE('',(#828,#211,#212,#213,#214,#215),#274,.T.);
#3677=ADVANCED_FACE('',(#829),#760,.F.);
#3678=ADVANCED_FACE('',(#830,#216),#275,.T.);
#3679=ADVANCED_FACE('',(#831,#217),#761,.F.);
#3680=ADVANCED_FACE('',(#832,#218),#276,.T.);
#3681=ADVANCED_FACE('',(#833),#3639,.F.);
#3682=ADVANCED_FACE('',(#834),#762,.T.);
#3683=ADVANCED_FACE('',(#835,#219,#220,#221,#222,#223),#277,.F.);
#3684=ADVANCED_FACE('',(#836,#224,#225,#226,#227,#228),#278,.T.);
#3685=ADVANCED_FACE('',(#837),#763,.F.);
#3686=ADVANCED_FACE('',(#838),#279,.F.);
#3687=ADVANCED_FACE('',(#839),#280,.F.);
#3688=ADVANCED_FACE('',(#840),#764,.F.);
#3689=ADVANCED_FACE('',(#841),#765,.F.);
#3690=ADVANCED_FACE('',(#842),#766,.F.);
#3691=ADVANCED_FACE('',(#843),#767,.F.);
#3692=ADVANCED_FACE('',(#844),#768,.F.);
#3693=ADVANCED_FACE('',(#845),#769,.F.);
#3694=ADVANCED_FACE('',(#846),#770,.F.);
#3695=ADVANCED_FACE('',(#847),#771,.F.);
#3696=ADVANCED_FACE('',(#848),#772,.F.);
#3697=ADVANCED_FACE('',(#849),#773,.F.);
#3698=ADVANCED_FACE('',(#850),#164,.F.);
#3699=ADVANCED_FACE('',(#851),#774,.F.);
#3700=ADVANCED_FACE('',(#852),#775,.F.);
#3701=ADVANCED_FACE('',(#853),#776,.F.);
#3702=ADVANCED_FACE('',(#854),#777,.T.);
#3703=ADVANCED_FACE('',(#855),#778,.T.);
#3704=ADVANCED_FACE('',(#856),#3640,.T.);
#3705=ADVANCED_FACE('',(#857),#3641,.T.);
#3706=ADVANCED_FACE('',(#858),#281,.T.);
#3707=ADVANCED_FACE('',(#859),#282,.T.);
#3708=ADVANCED_FACE('',(#860),#283,.T.);
#3709=ADVANCED_FACE('',(#861),#284,.T.);
#3710=ADVANCED_FACE('',(#862),#285,.F.);
#3711=ADVANCED_FACE('',(#863),#286,.F.);
#3712=ADVANCED_FACE('',(#864),#287,.F.);
#3713=ADVANCED_FACE('',(#865),#288,.F.);
#3714=ADVANCED_FACE('',(#866,#229),#289,.T.);
#3715=ADVANCED_FACE('',(#867),#779,.T.);
#3716=ADVANCED_FACE('',(#868,#230,#231),#290,.T.);
#3717=ADVANCED_FACE('',(#869),#780,.T.);
#3718=ADVANCED_FACE('',(#870),#165,.T.);
#3719=ADVANCED_FACE('',(#871),#291,.F.);
#3720=ADVANCED_FACE('',(#872,#232),#292,.F.);
#3721=ADVANCED_FACE('',(#873),#293,.F.);
#3722=ADVANCED_FACE('',(#874),#781,.F.);
#3723=ADVANCED_FACE('',(#875),#782,.T.);
#3724=ADVANCED_FACE('',(#876),#783,.T.);
#3725=ADVANCED_FACE('',(#877),#294,.T.);
#3726=ADVANCED_FACE('',(#878),#295,.F.);
#3727=ADVANCED_FACE('',(#879),#296,.F.);
#3728=ADVANCED_FACE('',(#880),#784,.T.);
#3729=ADVANCED_FACE('',(#881),#297,.F.);
#3730=ADVANCED_FACE('',(#882),#298,.F.);
#3731=ADVANCED_FACE('',(#883),#785,.T.);
#3732=ADVANCED_FACE('',(#884),#166,.T.);
#3733=ADVANCED_FACE('',(#885),#167,.T.);
#3734=ADVANCED_FACE('',(#886),#168,.T.);
#3735=ADVANCED_FACE('',(#887),#169,.T.);
#3736=ADVANCED_FACE('',(#888),#299,.T.);
#3737=ADVANCED_FACE('',(#889),#300,.T.);
#3738=ADVANCED_FACE('',(#890),#301,.T.);
#3739=ADVANCED_FACE('',(#891),#302,.T.);
#3740=ADVANCED_FACE('',(#892,#233),#303,.T.);
#3741=ADVANCED_FACE('',(#893),#786,.T.);
#3742=ADVANCED_FACE('',(#894,#234),#304,.T.);
#3743=ADVANCED_FACE('',(#895,#235,#236),#787,.T.);
#3744=ADVANCED_FACE('',(#896),#788,.F.);
#3745=ADVANCED_FACE('',(#897),#3642,.T.);
#3746=ADVANCED_FACE('',(#898),#305,.F.);
#3747=ADVANCED_FACE('',(#899),#306,.F.);
#3748=ADVANCED_FACE('',(#900),#307,.F.);
#3749=ADVANCED_FACE('',(#901),#308,.F.);
#3750=ADVANCED_FACE('',(#902),#309,.T.);
#3751=ADVANCED_FACE('',(#903),#789,.T.);
#3752=ADVANCED_FACE('',(#904),#310,.T.);
#3753=ADVANCED_FACE('',(#905,#237),#311,.T.);
#3754=ADVANCED_FACE('',(#906,#238),#312,.F.);
#3755=ADVANCED_FACE('',(#907,#239),#790,.T.);
#3756=ADVANCED_FACE('',(#908,#240),#791,.F.);
#3757=ADVANCED_FACE('',(#909),#170,.F.);
#3758=ADVANCED_FACE('',(#910),#171,.F.);
#3759=ADVANCED_FACE('',(#911),#172,.T.);
#3760=ADVANCED_FACE('',(#912),#313,.T.);
#3761=ADVANCED_FACE('',(#913),#314,.T.);
#3762=ADVANCED_FACE('',(#914,#241),#315,.T.);
#3763=ADVANCED_FACE('',(#915),#792,.F.);
#3764=ADVANCED_FACE('',(#916),#173,.F.);
#3765=ADVANCED_FACE('',(#917),#793,.F.);
#3766=ADVANCED_FACE('',(#918,#242),#316,.T.);
#3767=ADVANCED_FACE('',(#919),#174,.T.);
#3768=ADVANCED_FACE('',(#920,#243),#317,.T.);
#3769=ADVANCED_FACE('',(#921),#794,.T.);
#3770=ADVANCED_FACE('',(#922,#244,#245,#246,#247,#248),#318,.T.);
#3771=ADVANCED_FACE('',(#923),#795,.T.);
#3772=ADVANCED_FACE('',(#924,#249,#250,#251,#252,#253),#319,.T.);
#3773=ADVANCED_FACE('',(#925),#796,.T.);
#3774=ADVANCED_FACE('',(#926),#797,.F.);
#3775=ADVANCED_FACE('',(#927),#798,.F.);
#3776=ADVANCED_FACE('',(#928),#799,.F.);
#3777=ADVANCED_FACE('',(#929),#800,.F.);
#3778=ADVANCED_FACE('',(#930),#801,.F.);
#3779=ADVANCED_FACE('',(#931,#254),#320,.T.);
#3780=ADVANCED_FACE('',(#932),#802,.T.);
#3781=ADVANCED_FACE('',(#933,#255),#321,.T.);
#3782=ADVANCED_FACE('',(#934),#803,.T.);
#3783=ADVANCED_FACE('',(#935),#175,.F.);
#3784=ADVANCED_FACE('',(#936),#322,.F.);
#3785=ADVANCED_FACE('',(#937),#323,.F.);
#3786=ADVANCED_FACE('',(#938),#324,.F.);
#3787=ADVANCED_FACE('',(#939),#325,.F.);
#3788=ADVANCED_FACE('',(#940),#326,.F.);
#3789=ADVANCED_FACE('',(#941),#327,.F.);
#3790=ADVANCED_FACE('',(#942,#256),#328,.F.);
#3791=ADVANCED_FACE('',(#943),#804,.F.);
#3792=ADVANCED_FACE('',(#944,#257),#329,.T.);
#3793=ADVANCED_FACE('',(#945),#3643,.T.);
#3794=ADVANCED_FACE('',(#946),#3644,.T.);
#3795=ADVANCED_FACE('',(#947),#3645,.T.);
#3796=ADVANCED_FACE('',(#948),#3646,.T.);
#3797=ADVANCED_FACE('',(#949),#3647,.T.);
#3798=ADVANCED_FACE('',(#950),#3648,.T.);
#3799=ADVANCED_FACE('',(#951,#258),#330,.T.);
#3800=ADVANCED_FACE('',(#952),#176,.T.);
#3801=ADVANCED_FACE('',(#953),#805,.F.);
#3802=ADVANCED_FACE('',(#954,#259),#331,.T.);
#3803=ADVANCED_FACE('',(#955),#806,.F.);
#3804=ADVANCED_FACE('',(#956),#332,.T.);
#3805=ADVANCED_FACE('',(#957),#333,.F.);
#3806=ADVANCED_FACE('',(#958),#334,.F.);
#3807=ADVANCED_FACE('',(#959),#335,.F.);
#3808=ADVANCED_FACE('',(#960),#336,.F.);
#3809=ADVANCED_FACE('',(#961),#337,.F.);
#3810=ADVANCED_FACE('',(#962),#338,.F.);
#3811=ADVANCED_FACE('',(#963),#339,.F.);
#3812=ADVANCED_FACE('',(#964),#340,.T.);
#3813=ADVANCED_FACE('',(#965),#341,.F.);
#3814=ADVANCED_FACE('',(#966),#342,.T.);
#3815=ADVANCED_FACE('',(#967),#343,.F.);
#3816=ADVANCED_FACE('',(#968),#344,.T.);
#3817=ADVANCED_FACE('',(#969),#345,.F.);
#3818=ADVANCED_FACE('',(#970),#3649,.T.);
#3819=ADVANCED_FACE('',(#971),#346,.F.);
#3820=ADVANCED_FACE('',(#972),#347,.F.);
#3821=ADVANCED_FACE('',(#973,#260,#261,#262),#807,.T.);
#3822=ADVANCED_FACE('',(#974,#263),#348,.T.);
#3823=ADVANCED_FACE('',(#975,#264),#349,.F.);
#3824=ADVANCED_FACE('',(#976),#350,.F.);
#3825=ADVANCED_FACE('',(#977),#351,.F.);
#3826=ADVANCED_FACE('',(#978),#352,.F.);
#3827=ADVANCED_FACE('',(#979),#353,.F.);
#3828=ADVANCED_FACE('',(#980),#3650,.F.);
#3829=ADVANCED_FACE('',(#981),#3651,.F.);
#3830=ADVANCED_FACE('',(#982),#3652,.F.);
#3831=ADVANCED_FACE('',(#983),#3653,.F.);
#3832=ADVANCED_FACE('',(#984),#3654,.F.);
#3833=ADVANCED_FACE('',(#985),#3655,.F.);
#3834=ADVANCED_FACE('',(#986),#3656,.F.);
#3835=ADVANCED_FACE('',(#987),#3657,.F.);
#3836=ADVANCED_FACE('',(#988),#67,.F.);
#3837=ADVANCED_FACE('',(#989),#68,.F.);
#3838=ADVANCED_FACE('',(#990),#69,.F.);
#3839=ADVANCED_FACE('',(#991),#70,.F.);
#3840=ADVANCED_FACE('',(#992),#71,.F.);
#3841=ADVANCED_FACE('',(#993),#72,.F.);
#3842=ADVANCED_FACE('',(#994),#73,.F.);
#3843=ADVANCED_FACE('',(#995),#74,.F.);
#3844=ADVANCED_FACE('',(#996),#354,.F.);
#3845=ADVANCED_FACE('',(#997),#355,.F.);
#3846=ADVANCED_FACE('',(#998),#356,.F.);
#3847=ADVANCED_FACE('',(#999),#357,.F.);
#3848=ADVANCED_FACE('',(#1000),#358,.F.);
#3849=ADVANCED_FACE('',(#1001),#359,.F.);
#3850=ADVANCED_FACE('',(#1002,#265),#360,.F.);
#3851=ADVANCED_FACE('',(#1003,#266),#361,.T.);
#3852=ADVANCED_FACE('',(#1004),#808,.F.);
#3853=ADVANCED_FACE('',(#1005),#177,.T.);
#3854=ADVANCED_FACE('',(#1006),#178,.T.);
#3855=ADVANCED_FACE('',(#1007),#179,.T.);
#3856=ADVANCED_FACE('',(#1008),#180,.T.);
#3857=ADVANCED_FACE('',(#1009),#181,.T.);
#3858=ADVANCED_FACE('',(#1010),#182,.T.);
#3859=ADVANCED_FACE('',(#1011),#183,.T.);
#3860=ADVANCED_FACE('',(#1012),#184,.T.);
#3861=ADVANCED_FACE('',(#1013),#185,.T.);
#3862=ADVANCED_FACE('',(#1014),#186,.T.);
#3863=ADVANCED_FACE('',(#1015),#187,.T.);
#3864=ADVANCED_FACE('',(#1016),#188,.T.);
#3865=ADVANCED_FACE('',(#1017),#362,.F.);
#3866=ADVANCED_FACE('',(#1018),#363,.F.);
#3867=ADVANCED_FACE('',(#1019),#364,.F.);
#3868=ADVANCED_FACE('',(#1020),#365,.F.);
#3869=ADVANCED_FACE('',(#1021),#366,.F.);
#3870=ADVANCED_FACE('',(#1022),#367,.F.);
#3871=ADVANCED_FACE('',(#1023),#809,.T.);
#3872=ADVANCED_FACE('',(#1024),#368,.F.);
#3873=ADVANCED_FACE('',(#1025,#267),#369,.F.);
#3874=ADVANCED_FACE('',(#1026),#189,.T.);
#3875=ADVANCED_FACE('',(#1027),#190,.T.);
#3876=ADVANCED_FACE('',(#1028),#191,.T.);
#3877=ADVANCED_FACE('',(#1029),#192,.T.);
#3878=ADVANCED_FACE('',(#1030),#193,.T.);
#3879=ADVANCED_FACE('',(#1031),#194,.T.);
#3880=ADVANCED_FACE('',(#1032),#370,.T.);
#3881=CLOSED_SHELL('',(#3658,#3659,#3660,#3661,#3662,#3663,#3664,#3665,
#3666,#3667,#3668,#3669,#3670,#3671,#3672,#3673,#3674,#3675,#3676,#3677,
#3678,#3679,#3680,#3681,#3682,#3683,#3684,#3685,#3686,#3687,#3688,#3689,
#3690,#3691,#3692,#3693,#3694,#3695,#3696,#3697,#3698,#3699,#3700,#3701,
#3702,#3703,#3704,#3705));
#3882=CLOSED_SHELL('',(#3706,#3707,#3708,#3709,#3710,#3711,#3712,#3713,
#3714,#3715,#3716,#3717,#3718,#3719,#3720,#3721,#3722,#3723,#3724,#3725,
#3726,#3727,#3728,#3729,#3730,#3731,#3732,#3733,#3734,#3735));
#3883=CLOSED_SHELL('',(#3736,#3737,#3738,#3739,#3740,#3741,#3742,#3743,
#3744,#3745,#3746,#3747,#3748,#3749,#3750,#3751,#3752));
#3884=CLOSED_SHELL('',(#3753,#3754,#3755,#3756,#3757,#3758));
#3885=CLOSED_SHELL('',(#3759,#3760,#3761));
#3886=CLOSED_SHELL('',(#3762,#3763,#3764,#3765,#3766,#3767,#3768,#3769,
#3770,#3771,#3772,#3773,#3774,#3775,#3776,#3777));
#3887=CLOSED_SHELL('',(#3778,#3779,#3780,#3781,#3782,#3783));
#3888=CLOSED_SHELL('',(#3784,#3785,#3786,#3787,#3788,#3789,#3790,#3791,
#3792,#3793,#3794,#3795,#3796,#3797,#3798,#3799,#3800,#3801,#3802,#3803));
#3889=CLOSED_SHELL('',(#3804,#3805,#3806,#3807,#3808,#3809,#3810,#3811,
#3812,#3813,#3814,#3815,#3816,#3817,#3818,#3819,#3820,#3821,#3822,#3823,
#3824,#3825,#3826,#3827,#3828,#3829,#3830,#3831,#3832,#3833,#3834,#3835,
#3836,#3837,#3838,#3839,#3840,#3841,#3842,#3843));
#3890=CLOSED_SHELL('',(#3844,#3845,#3846,#3847,#3848,#3849,#3850,#3851,
#3852,#3853,#3854,#3855,#3856,#3857,#3858,#3859,#3860,#3861,#3862,#3863,
#3864));
#3891=CLOSED_SHELL('',(#3865,#3866,#3867,#3868,#3869,#3870,#3871,#3872,
#3873,#3874,#3875,#3876,#3877,#3878,#3879,#3880));
#3892=DERIVED_UNIT_ELEMENT(#3914,1.);
#3893=DERIVED_UNIT_ELEMENT(#9670,-3.);
#3894=DERIVED_UNIT_ELEMENT(#3914,1.);
#3895=DERIVED_UNIT_ELEMENT(#9670,-3.);
#3896=DERIVED_UNIT_ELEMENT(#3914,1.);
#3897=DERIVED_UNIT_ELEMENT(#9670,-3.);
#3898=DERIVED_UNIT_ELEMENT(#3914,1.);
#3899=DERIVED_UNIT_ELEMENT(#9670,-3.);
#3900=DERIVED_UNIT_ELEMENT(#3914,1.);
#3901=DERIVED_UNIT_ELEMENT(#9670,-3.);
#3902=DERIVED_UNIT_ELEMENT(#3914,1.);
#3903=DERIVED_UNIT_ELEMENT(#9670,-3.);
#3904=DERIVED_UNIT_ELEMENT(#3914,1.);
#3905=DERIVED_UNIT_ELEMENT(#9670,-3.);
#3906=DERIVED_UNIT_ELEMENT(#3914,1.);
#3907=DERIVED_UNIT_ELEMENT(#9670,-3.);
#3908=DERIVED_UNIT_ELEMENT(#3914,1.);
#3909=DERIVED_UNIT_ELEMENT(#9670,-3.);
#3910=DERIVED_UNIT_ELEMENT(#3914,1.);
#3911=DERIVED_UNIT_ELEMENT(#9670,-3.);
#3912=DERIVED_UNIT_ELEMENT(#3914,1.);
#3913=DERIVED_UNIT_ELEMENT(#9670,-3.);
#3914=(
MASS_UNIT()
NAMED_UNIT(*)
SI_UNIT(.KILO.,.GRAM.)
);
#3915=DERIVED_UNIT((#3892,#3893));
#3916=DERIVED_UNIT((#3894,#3895));
#3917=DERIVED_UNIT((#3896,#3897));
#3918=DERIVED_UNIT((#3898,#3899));
#3919=DERIVED_UNIT((#3900,#3901));
#3920=DERIVED_UNIT((#3902,#3903));
#3921=DERIVED_UNIT((#3904,#3905));
#3922=DERIVED_UNIT((#3906,#3907));
#3923=DERIVED_UNIT((#3908,#3909));
#3924=DERIVED_UNIT((#3910,#3911));
#3925=DERIVED_UNIT((#3912,#3913));
#3926=MEASURE_REPRESENTATION_ITEM('density measure',
POSITIVE_RATIO_MEASURE(7200.),#3915);
#3927=MEASURE_REPRESENTATION_ITEM('density measure',
POSITIVE_RATIO_MEASURE(8027.),#3916);
#3928=MEASURE_REPRESENTATION_ITEM('density measure',
POSITIVE_RATIO_MEASURE(8027.),#3917);
#3929=MEASURE_REPRESENTATION_ITEM('density measure',
POSITIVE_RATIO_MEASURE(7200.),#3918);
#3930=MEASURE_REPRESENTATION_ITEM('density measure',
POSITIVE_RATIO_MEASURE(7700.),#3919);
#3931=MEASURE_REPRESENTATION_ITEM('density measure',
POSITIVE_RATIO_MEASURE(7200.),#3920);
#3932=MEASURE_REPRESENTATION_ITEM('density measure',
POSITIVE_RATIO_MEASURE(7800.),#3921);
#3933=MEASURE_REPRESENTATION_ITEM('density measure',
POSITIVE_RATIO_MEASURE(7700.),#3922);
#3934=MEASURE_REPRESENTATION_ITEM('density measure',
POSITIVE_RATIO_MEASURE(8027.),#3923);
#3935=MEASURE_REPRESENTATION_ITEM('density measure',
POSITIVE_RATIO_MEASURE(7800.),#3924);
#3936=MEASURE_REPRESENTATION_ITEM('density measure',
POSITIVE_RATIO_MEASURE(7800.),#3925);
#3937=PROPERTY_DEFINITION_REPRESENTATION(#3992,#3959);
#3938=PROPERTY_DEFINITION_REPRESENTATION(#3993,#3960);
#3939=PROPERTY_DEFINITION_REPRESENTATION(#3994,#3961);
#3940=PROPERTY_DEFINITION_REPRESENTATION(#3995,#3962);
#3941=PROPERTY_DEFINITION_REPRESENTATION(#3996,#3963);
#3942=PROPERTY_DEFINITION_REPRESENTATION(#3997,#3964);
#3943=PROPERTY_DEFINITION_REPRESENTATION(#3998,#3965);
#3944=PROPERTY_DEFINITION_REPRESENTATION(#3999,#3966);
#3945=PROPERTY_DEFINITION_REPRESENTATION(#4000,#3967);
#3946=PROPERTY_DEFINITION_REPRESENTATION(#4001,#3968);
#3947=PROPERTY_DEFINITION_REPRESENTATION(#4002,#3969);
#3948=PROPERTY_DEFINITION_REPRESENTATION(#4003,#3970);
#3949=PROPERTY_DEFINITION_REPRESENTATION(#4004,#3971);
#3950=PROPERTY_DEFINITION_REPRESENTATION(#4005,#3972);
#3951=PROPERTY_DEFINITION_REPRESENTATION(#4006,#3973);
#3952=PROPERTY_DEFINITION_REPRESENTATION(#4007,#3974);
#3953=PROPERTY_DEFINITION_REPRESENTATION(#4008,#3975);
#3954=PROPERTY_DEFINITION_REPRESENTATION(#4009,#3976);
#3955=PROPERTY_DEFINITION_REPRESENTATION(#4010,#3977);
#3956=PROPERTY_DEFINITION_REPRESENTATION(#4011,#3978);
#3957=PROPERTY_DEFINITION_REPRESENTATION(#4012,#3979);
#3958=PROPERTY_DEFINITION_REPRESENTATION(#4013,#3980);
#3959=REPRESENTATION('material name',(#3981),#9657);
#3960=REPRESENTATION('density',(#3926),#9657);
#3961=REPRESENTATION('material name',(#3982),#9658);
#3962=REPRESENTATION('density',(#3927),#9658);
#3963=REPRESENTATION('material name',(#3983),#9659);
#3964=REPRESENTATION('density',(#3928),#9659);
#3965=REPRESENTATION('material name',(#3984),#9660);
#3966=REPRESENTATION('density',(#3929),#9660);
#3967=REPRESENTATION('material name',(#3985),#9661);
#3968=REPRESENTATION('density',(#3930),#9661);
#3969=REPRESENTATION('material name',(#3986),#9662);
#3970=REPRESENTATION('density',(#3931),#9662);
#3971=REPRESENTATION('material name',(#3987),#9663);
#3972=REPRESENTATION('density',(#3932),#9663);
#3973=REPRESENTATION('material name',(#3988),#9664);
#3974=REPRESENTATION('density',(#3933),#9664);
#3975=REPRESENTATION('material name',(#3989),#9665);
#3976=REPRESENTATION('density',(#3934),#9665);
#3977=REPRESENTATION('material name',(#3990),#9666);
#3978=REPRESENTATION('density',(#3935),#9666);
#3979=REPRESENTATION('material name',(#3991),#9667);
#3980=REPRESENTATION('density',(#3936),#9667);
#3981=DESCRIPTIVE_REPRESENTATION_ITEM('Gray Cast Iron','Gray Cast Iron');
#3982=DESCRIPTIVE_REPRESENTATION_ITEM('AISI Type 316L stainless steel',
'AISI Type 316L stainless steel');
#3983=DESCRIPTIVE_REPRESENTATION_ITEM('AISI Type 316L stainless steel',
'AISI Type 316L stainless steel');
#3984=DESCRIPTIVE_REPRESENTATION_ITEM('Gray Cast Iron','Gray Cast Iron');
#3985=DESCRIPTIVE_REPRESENTATION_ITEM('Alloy Steel','Alloy Steel');
#3986=DESCRIPTIVE_REPRESENTATION_ITEM('Gray Cast Iron','Gray Cast Iron');
#3987=DESCRIPTIVE_REPRESENTATION_ITEM('Cast Carbon Steel',
'Cast Carbon Steel');
#3988=DESCRIPTIVE_REPRESENTATION_ITEM('Alloy Steel','Alloy Steel');
#3989=DESCRIPTIVE_REPRESENTATION_ITEM('AISI Type 316L stainless steel',
'AISI Type 316L stainless steel');
#3990=DESCRIPTIVE_REPRESENTATION_ITEM('Cast Carbon Steel',
'Cast Carbon Steel');
#3991=DESCRIPTIVE_REPRESENTATION_ITEM('Cast Carbon Steel',
'Cast Carbon Steel');
#3992=PROPERTY_DEFINITION('material property','material name',#9725);
#3993=PROPERTY_DEFINITION('material property','density of part',#9725);
#3994=PROPERTY_DEFINITION('material property','material name',#9726);
#3995=PROPERTY_DEFINITION('material property','density of part',#9726);
#3996=PROPERTY_DEFINITION('material property','material name',#9727);
#3997=PROPERTY_DEFINITION('material property','density of part',#9727);
#3998=PROPERTY_DEFINITION('material property','material name',#9728);
#3999=PROPERTY_DEFINITION('material property','density of part',#9728);
#4000=PROPERTY_DEFINITION('material property','material name',#9729);
#4001=PROPERTY_DEFINITION('material property','density of part',#9729);
#4002=PROPERTY_DEFINITION('material property','material name',#9730);
#4003=PROPERTY_DEFINITION('material property','density of part',#9730);
#4004=PROPERTY_DEFINITION('material property','material name',#9731);
#4005=PROPERTY_DEFINITION('material property','density of part',#9731);
#4006=PROPERTY_DEFINITION('material property','material name',#9732);
#4007=PROPERTY_DEFINITION('material property','density of part',#9732);
#4008=PROPERTY_DEFINITION('material property','material name',#9733);
#4009=PROPERTY_DEFINITION('material property','density of part',#9733);
#4010=PROPERTY_DEFINITION('material property','material name',#9734);
#4011=PROPERTY_DEFINITION('material property','density of part',#9734);
#4012=PROPERTY_DEFINITION('material property','material name',#9735);
#4013=PROPERTY_DEFINITION('material property','density of part',#9735);
#4014=AXIS2_PLACEMENT_3D('',#5570,#4469,#4470);
#4015=AXIS2_PLACEMENT_3D('',#5571,#4471,#4472);
#4016=AXIS2_PLACEMENT_3D('',#5572,#4473,#4474);
#4017=AXIS2_PLACEMENT_3D('',#5575,#4475,#4476);
#4018=AXIS2_PLACEMENT_3D('',#5586,#4477,#4478);
#4019=AXIS2_PLACEMENT_3D('',#5588,#4479,#4480);
#4020=AXIS2_PLACEMENT_3D('',#5599,#4481,#4482);
#4021=AXIS2_PLACEMENT_3D('',#5689,#4485,#4486);
#4022=AXIS2_PLACEMENT_3D('',#5775,#4488,#4489);
#4023=AXIS2_PLACEMENT_3D('',#5778,#4490,#4491);
#4024=AXIS2_PLACEMENT_3D('',#5779,#4492,#4493);
#4025=AXIS2_PLACEMENT_3D('',#5781,#4494,#4495);
#4026=AXIS2_PLACEMENT_3D('',#5783,#4496,#4497);
#4027=AXIS2_PLACEMENT_3D('',#5991,#4498,#4499);
#4028=AXIS2_PLACEMENT_3D('',#5992,#4500,#4501);
#4029=AXIS2_PLACEMENT_3D('',#5994,#4502,#4503);
#4030=AXIS2_PLACEMENT_3D('',#5998,#4506,#4507);
#4031=AXIS2_PLACEMENT_3D('',#6000,#4508,#4509);
#4032=AXIS2_PLACEMENT_3D('',#6002,#4510,#4511);
#4033=AXIS2_PLACEMENT_3D('',#6004,#4512,#4513);
#4034=AXIS2_PLACEMENT_3D('',#6005,#4514,#4515);
#4035=AXIS2_PLACEMENT_3D('',#6007,#4516,#4517);
#4036=AXIS2_PLACEMENT_3D('',#6009,#4518,#4519);
#4037=AXIS2_PLACEMENT_3D('',#6010,#4520,#4521);
#4038=AXIS2_PLACEMENT_3D('',#6013,#4522,#4523);
#4039=AXIS2_PLACEMENT_3D('',#6014,#4524,#4525);
#4040=AXIS2_PLACEMENT_3D('',#6016,#4527,#4528);
#4041=AXIS2_PLACEMENT_3D('',#6019,#4530,#4531);
#4042=AXIS2_PLACEMENT_3D('',#6020,#4532,#4533);
#4043=AXIS2_PLACEMENT_3D('',#6022,#4534,#4535);
#4044=AXIS2_PLACEMENT_3D('',#6023,#4536,#4537);
#4045=AXIS2_PLACEMENT_3D('',#6026,#4539,#4540);
#4046=AXIS2_PLACEMENT_3D('',#6027,#4541,#4542);
#4047=AXIS2_PLACEMENT_3D('',#6029,#4543,#4544);
#4048=AXIS2_PLACEMENT_3D('',#6031,#4545,#4546);
#4049=AXIS2_PLACEMENT_3D('',#6033,#4547,#4548);
#4050=AXIS2_PLACEMENT_3D('',#6035,#4549,#4550);
#4051=AXIS2_PLACEMENT_3D('',#6037,#4551,#4552);
#4052=AXIS2_PLACEMENT_3D('',#6038,#4553,#4554);
#4053=AXIS2_PLACEMENT_3D('',#6042,#4556,#4557);
#4054=AXIS2_PLACEMENT_3D('',#6043,#4558,#4559);
#4055=AXIS2_PLACEMENT_3D('',#6044,#4560,#4561);
#4056=AXIS2_PLACEMENT_3D('',#6046,#4562,#4563);
#4057=AXIS2_PLACEMENT_3D('',#6048,#4564,#4565);
#4058=AXIS2_PLACEMENT_3D('',#6050,#4566,#4567);
#4059=AXIS2_PLACEMENT_3D('',#6052,#4568,#4569);
#4060=AXIS2_PLACEMENT_3D('',#6054,#4570,#4571);
#4061=AXIS2_PLACEMENT_3D('',#6056,#4572,#4573);
#4062=AXIS2_PLACEMENT_3D('',#6057,#4574,#4575);
#4063=AXIS2_PLACEMENT_3D('',#6061,#4577,#4578);
#4064=AXIS2_PLACEMENT_3D('',#6062,#4579,#4580);
#4065=AXIS2_PLACEMENT_3D('',#6063,#4581,#4582);
#4066=AXIS2_PLACEMENT_3D('',#6065,#4583,#4584);
#4067=AXIS2_PLACEMENT_3D('',#6066,#4585,#4586);
#4068=AXIS2_PLACEMENT_3D('',#6067,#4587,#4588);
#4069=AXIS2_PLACEMENT_3D('',#6069,#4589,#4590);
#4070=AXIS2_PLACEMENT_3D('',#6070,#4591,#4592);
#4071=AXIS2_PLACEMENT_3D('',#6072,#4593,#4594);
#4072=AXIS2_PLACEMENT_3D('',#6074,#4595,#4596);
#4073=AXIS2_PLACEMENT_3D('',#6075,#4597,#4598);
#4074=AXIS2_PLACEMENT_3D('',#6076,#4599,#4600);
#4075=AXIS2_PLACEMENT_3D('',#6077,#4601,#4602);
#4076=AXIS2_PLACEMENT_3D('',#6079,#4604,#4605);
#4077=AXIS2_PLACEMENT_3D('',#6083,#4608,#4609);
#4078=AXIS2_PLACEMENT_3D('',#6085,#4611,#4612);
#4079=AXIS2_PLACEMENT_3D('',#6087,#4613,#4614);
#4080=AXIS2_PLACEMENT_3D('',#6089,#4615,#4616);
#4081=AXIS2_PLACEMENT_3D('',#6091,#4617,#4618);
#4082=AXIS2_PLACEMENT_3D('',#6093,#4619,#4620);
#4083=AXIS2_PLACEMENT_3D('',#6095,#4621,#4622);
#4084=AXIS2_PLACEMENT_3D('',#6096,#4623,#4624);
#4085=AXIS2_PLACEMENT_3D('',#6099,#4625,#4626);
#4086=AXIS2_PLACEMENT_3D('',#6100,#4627,#4628);
#4087=AXIS2_PLACEMENT_3D('',#6103,#4630,#4631);
#4088=AXIS2_PLACEMENT_3D('',#6104,#4632,#4633);
#4089=AXIS2_PLACEMENT_3D('',#6106,#4634,#4635);
#4090=AXIS2_PLACEMENT_3D('',#6107,#4636,#4637);
#4091=AXIS2_PLACEMENT_3D('',#6110,#4639,#4640);
#4092=AXIS2_PLACEMENT_3D('',#6181,#4641,#4642);
#4093=AXIS2_PLACEMENT_3D('',#6183,#4643,#4644);
#4094=AXIS2_PLACEMENT_3D('',#6184,#4645,#4646);
#4095=AXIS2_PLACEMENT_3D('',#6185,#4647,#4648);
#4096=AXIS2_PLACEMENT_3D('',#6186,#4649,#4650);
#4097=AXIS2_PLACEMENT_3D('',#6188,#4651,#4652);
#4098=AXIS2_PLACEMENT_3D('',#6191,#4654,#4655);
#4099=AXIS2_PLACEMENT_3D('',#6192,#4656,#4657);
#4100=AXIS2_PLACEMENT_3D('',#6194,#4658,#4659);
#4101=AXIS2_PLACEMENT_3D('',#6196,#4660,#4661);
#4102=AXIS2_PLACEMENT_3D('',#6198,#4662,#4663);
#4103=AXIS2_PLACEMENT_3D('',#6200,#4664,#4665);
#4104=AXIS2_PLACEMENT_3D('',#6201,#4666,#4667);
#4105=AXIS2_PLACEMENT_3D('',#6203,#4668,#4669);
#4106=AXIS2_PLACEMENT_3D('',#6205,#4670,#4671);
#4107=AXIS2_PLACEMENT_3D('',#6207,#4672,#4673);
#4108=AXIS2_PLACEMENT_3D('',#6209,#4674,#4675);
#4109=AXIS2_PLACEMENT_3D('',#6211,#4676,#4677);
#4110=AXIS2_PLACEMENT_3D('',#6212,#4678,#4679);
#4111=AXIS2_PLACEMENT_3D('',#6215,#4682,#4683);
#4112=AXIS2_PLACEMENT_3D('',#6217,#4685,#4686);
#4113=AXIS2_PLACEMENT_3D('',#6219,#4688,#4689);
#4114=AXIS2_PLACEMENT_3D('',#6221,#4691,#4692);
#4115=AXIS2_PLACEMENT_3D('',#6223,#4694,#4695);
#4116=AXIS2_PLACEMENT_3D('',#6225,#4697,#4698);
#4117=AXIS2_PLACEMENT_3D('',#6227,#4700,#4701);
#4118=AXIS2_PLACEMENT_3D('',#6229,#4703,#4704);
#4119=AXIS2_PLACEMENT_3D('',#6231,#4706,#4707);
#4120=AXIS2_PLACEMENT_3D('',#6233,#4709,#4710);
#4121=AXIS2_PLACEMENT_3D('',#6235,#4712,#4713);
#4122=AXIS2_PLACEMENT_3D('',#6237,#4715,#4716);
#4123=AXIS2_PLACEMENT_3D('',#6241,#4718,#4719);
#4124=AXIS2_PLACEMENT_3D('',#6242,#4720,#4721);
#4125=AXIS2_PLACEMENT_3D('',#6243,#4722,#4723);
#4126=AXIS2_PLACEMENT_3D('',#6246,#4725,#4726);
#4127=AXIS2_PLACEMENT_3D('',#6248,#4728,#4729);
#4128=AXIS2_PLACEMENT_3D('',#6250,#4731,#4732);
#4129=AXIS2_PLACEMENT_3D('',#6252,#4734,#4735);
#4130=AXIS2_PLACEMENT_3D('',#6253,#4736,#4737);
#4131=AXIS2_PLACEMENT_3D('',#6254,#4738,#4739);
#4132=AXIS2_PLACEMENT_3D('',#6255,#4740,#4741);
#4133=AXIS2_PLACEMENT_3D('',#6256,#4742,#4743);
#4134=AXIS2_PLACEMENT_3D('',#6257,#4744,#4745);
#4135=AXIS2_PLACEMENT_3D('',#6258,#4746,#4747);
#4136=AXIS2_PLACEMENT_3D('',#6259,#4748,#4749);
#4137=AXIS2_PLACEMENT_3D('',#6262,#4750,#4751);
#4138=AXIS2_PLACEMENT_3D('',#6266,#4754,#4755);
#4139=AXIS2_PLACEMENT_3D('',#6272,#4758,#4759);
#4140=AXIS2_PLACEMENT_3D('',#6273,#4760,#4761);
#4141=AXIS2_PLACEMENT_3D('',#6279,#4764,#4765);
#4142=AXIS2_PLACEMENT_3D('',#6280,#4766,#4767);
#4143=AXIS2_PLACEMENT_3D('',#6283,#4768,#4769);
#4144=AXIS2_PLACEMENT_3D('',#6287,#4772,#4773);
#4145=AXIS2_PLACEMENT_3D('',#6297,#4777,#4778);
#4146=AXIS2_PLACEMENT_3D('',#6307,#4782,#4783);
#4147=AXIS2_PLACEMENT_3D('',#6317,#4787,#4788);
#4148=AXIS2_PLACEMENT_3D('',#6327,#4792,#4793);
#4149=AXIS2_PLACEMENT_3D('',#6329,#4794,#4795);
#4150=AXIS2_PLACEMENT_3D('',#6331,#4796,#4797);
#4151=AXIS2_PLACEMENT_3D('',#6332,#4798,#4799);
#4152=AXIS2_PLACEMENT_3D('',#6337,#4801,#4802);
#4153=AXIS2_PLACEMENT_3D('',#6340,#4804,#4805);
#4154=AXIS2_PLACEMENT_3D('',#6344,#4807,#4808);
#4155=AXIS2_PLACEMENT_3D('',#6348,#4810,#4811);
#4156=AXIS2_PLACEMENT_3D('',#6351,#4813,#4814);
#4157=AXIS2_PLACEMENT_3D('',#6352,#4815,#4816);
#4158=AXIS2_PLACEMENT_3D('',#6354,#4817,#4818);
#4159=AXIS2_PLACEMENT_3D('',#6357,#4821,#4822);
#4160=AXIS2_PLACEMENT_3D('',#6360,#4823,#4824);
#4161=AXIS2_PLACEMENT_3D('',#6361,#4825,#4826);
#4162=AXIS2_PLACEMENT_3D('',#6363,#4828,#4829);
#4163=AXIS2_PLACEMENT_3D('',#6366,#4831,#4832);
#4164=AXIS2_PLACEMENT_3D('',#6367,#4833,#4834);
#4165=AXIS2_PLACEMENT_3D('',#6368,#4835,#4836);
#4166=AXIS2_PLACEMENT_3D('',#6369,#4837,#4838);
#4167=AXIS2_PLACEMENT_3D('',#6370,#4839,#4840);
#4168=AXIS2_PLACEMENT_3D('',#6371,#4841,#4842);
#4169=AXIS2_PLACEMENT_3D('',#6373,#4844,#4845);
#4170=AXIS2_PLACEMENT_3D('',#6376,#4847,#4848);
#4171=AXIS2_PLACEMENT_3D('',#6377,#4849,#4850);
#4172=AXIS2_PLACEMENT_3D('',#6378,#4851,#4852);
#4173=AXIS2_PLACEMENT_3D('',#6380,#4854,#4855);
#4174=AXIS2_PLACEMENT_3D('',#6381,#4856,#4857);
#4175=AXIS2_PLACEMENT_3D('',#6382,#4858,#4859);
#4176=AXIS2_PLACEMENT_3D('',#6383,#4860,#4861);
#4177=AXIS2_PLACEMENT_3D('',#6384,#4862,#4863);
#4178=AXIS2_PLACEMENT_3D('',#6388,#4865,#4866);
#4179=AXIS2_PLACEMENT_3D('',#6390,#4868,#4869);
#4180=AXIS2_PLACEMENT_3D('',#6394,#4871,#4872);
#4181=AXIS2_PLACEMENT_3D('',#6396,#4874,#4875);
#4182=AXIS2_PLACEMENT_3D('',#6397,#4876,#4877);
#4183=AXIS2_PLACEMENT_3D('',#6403,#4879,#4880);
#4184=AXIS2_PLACEMENT_3D('',#6409,#4882,#4883);
#4185=AXIS2_PLACEMENT_3D('',#6410,#4884,#4885);
#4186=AXIS2_PLACEMENT_3D('',#6411,#4886,#4887);
#4187=AXIS2_PLACEMENT_3D('',#6417,#4889,#4890);
#4188=AXIS2_PLACEMENT_3D('',#6423,#4892,#4893);
#4189=AXIS2_PLACEMENT_3D('',#6424,#4894,#4895);
#4190=AXIS2_PLACEMENT_3D('',#6425,#4896,#4897);
#4191=AXIS2_PLACEMENT_3D('',#6426,#4898,#4899);
#4192=AXIS2_PLACEMENT_3D('',#6427,#4900,#4901);
#4193=AXIS2_PLACEMENT_3D('',#6428,#4902,#4903);
#4194=AXIS2_PLACEMENT_3D('',#6429,#4904,#4905);
#4195=AXIS2_PLACEMENT_3D('',#6430,#4906,#4907);
#4196=AXIS2_PLACEMENT_3D('',#6433,#4908,#4909);
#4197=AXIS2_PLACEMENT_3D('',#6437,#4912,#4913);
#4198=AXIS2_PLACEMENT_3D('',#6439,#4914,#4915);
#4199=AXIS2_PLACEMENT_3D('',#6443,#4918,#4919);
#4200=AXIS2_PLACEMENT_3D('',#6445,#4920,#4921);
#4201=AXIS2_PLACEMENT_3D('',#6449,#4924,#4925);
#4202=AXIS2_PLACEMENT_3D('',#6451,#4926,#4927);
#4203=AXIS2_PLACEMENT_3D('',#6452,#4928,#4929);
#4204=AXIS2_PLACEMENT_3D('',#6454,#4930,#4931);
#4205=AXIS2_PLACEMENT_3D('',#6463,#4936,#4937);
#4206=AXIS2_PLACEMENT_3D('',#6465,#4938,#4939);
#4207=AXIS2_PLACEMENT_3D('',#6467,#4941,#4942);
#4208=AXIS2_PLACEMENT_3D('',#6469,#4943,#4944);
#4209=AXIS2_PLACEMENT_3D('',#6470,#4945,#4946);
#4210=AXIS2_PLACEMENT_3D('',#6472,#4947,#4948);
#4211=AXIS2_PLACEMENT_3D('',#6550,#4950,#4951);
#4212=AXIS2_PLACEMENT_3D('',#6552,#4953,#4954);
#4213=AXIS2_PLACEMENT_3D('',#6553,#4955,#4956);
#4214=AXIS2_PLACEMENT_3D('',#6554,#4957,#4958);
#4215=AXIS2_PLACEMENT_3D('',#6559,#4962,#4963);
#4216=AXIS2_PLACEMENT_3D('',#6561,#4965,#4966);
#4217=AXIS2_PLACEMENT_3D('',#6563,#4968,#4969);
#4218=AXIS2_PLACEMENT_3D('',#6565,#4971,#4972);
#4219=AXIS2_PLACEMENT_3D('',#6566,#4973,#4974);
#4220=AXIS2_PLACEMENT_3D('',#6567,#4975,#4976);
#4221=AXIS2_PLACEMENT_3D('',#6570,#4978,#4979);
#4222=AXIS2_PLACEMENT_3D('',#6571,#4980,#4981);
#4223=AXIS2_PLACEMENT_3D('',#6572,#4982,#4983);
#4224=AXIS2_PLACEMENT_3D('',#6573,#4984,#4985);
#4225=AXIS2_PLACEMENT_3D('',#6575,#4986,#4987);
#4226=AXIS2_PLACEMENT_3D('',#6577,#4988,#4989);
#4227=AXIS2_PLACEMENT_3D('',#6578,#4990,#4991);
#4228=AXIS2_PLACEMENT_3D('',#6580,#4992,#4993);
#4229=AXIS2_PLACEMENT_3D('',#6582,#4994,#4995);
#4230=AXIS2_PLACEMENT_3D('',#6583,#4996,#4997);
#4231=AXIS2_PLACEMENT_3D('',#6672,#5000,#5001);
#4232=AXIS2_PLACEMENT_3D('',#6761,#5004,#5005);
#4233=AXIS2_PLACEMENT_3D('',#6763,#5007,#5008);
#4234=AXIS2_PLACEMENT_3D('',#6765,#5010,#5011);
#4235=AXIS2_PLACEMENT_3D('',#6766,#5012,#5013);
#4236=AXIS2_PLACEMENT_3D('',#6768,#5014,#5015);
#4237=AXIS2_PLACEMENT_3D('',#6771,#5017,#5018);
#4238=AXIS2_PLACEMENT_3D('',#6772,#5019,#5020);
#4239=AXIS2_PLACEMENT_3D('',#6773,#5021,#5022);
#4240=AXIS2_PLACEMENT_3D('',#6774,#5023,#5024);
#4241=AXIS2_PLACEMENT_3D('',#6775,#5025,#5026);
#4242=AXIS2_PLACEMENT_3D('',#6777,#5027,#5028);
#4243=AXIS2_PLACEMENT_3D('',#6779,#5029,#5030);
#4244=AXIS2_PLACEMENT_3D('',#6780,#5031,#5032);
#4245=AXIS2_PLACEMENT_3D('',#6784,#5034,#5035);
#4246=AXIS2_PLACEMENT_3D('',#6785,#5036,#5037);
#4247=AXIS2_PLACEMENT_3D('',#6786,#5038,#5039);
#4248=AXIS2_PLACEMENT_3D('',#6789,#5040,#5041);
#4249=AXIS2_PLACEMENT_3D('',#6790,#5042,#5043);
#4250=AXIS2_PLACEMENT_3D('',#6792,#5045,#5046);
#4251=AXIS2_PLACEMENT_3D('',#6795,#5048,#5049);
#4252=AXIS2_PLACEMENT_3D('',#6796,#5050,#5051);
#4253=AXIS2_PLACEMENT_3D('',#6798,#5052,#5053);
#4254=AXIS2_PLACEMENT_3D('',#6799,#5054,#5055);
#4255=AXIS2_PLACEMENT_3D('',#6801,#5056,#5057);
#4256=AXIS2_PLACEMENT_3D('',#6803,#5059,#5060);
#4257=AXIS2_PLACEMENT_3D('',#6805,#5061,#5062);
#4258=AXIS2_PLACEMENT_3D('',#6806,#5063,#5064);
#4259=AXIS2_PLACEMENT_3D('',#6809,#5066,#5067);
#4260=AXIS2_PLACEMENT_3D('',#6810,#5068,#5069);
#4261=AXIS2_PLACEMENT_3D('',#6812,#5070,#5071);
#4262=AXIS2_PLACEMENT_3D('',#6814,#5072,#5073);
#4263=AXIS2_PLACEMENT_3D('',#6816,#5074,#5075);
#4264=AXIS2_PLACEMENT_3D('',#6818,#5076,#5077);
#4265=AXIS2_PLACEMENT_3D('',#6820,#5078,#5079);
#4266=AXIS2_PLACEMENT_3D('',#6821,#5080,#5081);
#4267=AXIS2_PLACEMENT_3D('',#6824,#5083,#5084);
#4268=AXIS2_PLACEMENT_3D('',#6825,#5085,#5086);
#4269=AXIS2_PLACEMENT_3D('',#6827,#5087,#5088);
#4270=AXIS2_PLACEMENT_3D('',#6829,#5089,#5090);
#4271=AXIS2_PLACEMENT_3D('',#6831,#5091,#5092);
#4272=AXIS2_PLACEMENT_3D('',#6833,#5093,#5094);
#4273=AXIS2_PLACEMENT_3D('',#6835,#5095,#5096);
#4274=AXIS2_PLACEMENT_3D('',#6836,#5097,#5098);
#4275=AXIS2_PLACEMENT_3D('',#6838,#5100,#5101);
#4276=AXIS2_PLACEMENT_3D('',#6840,#5103,#5104);
#4277=AXIS2_PLACEMENT_3D('',#6842,#5106,#5107);
#4278=AXIS2_PLACEMENT_3D('',#6844,#5109,#5110);
#4279=AXIS2_PLACEMENT_3D('',#6846,#5112,#5113);
#4280=AXIS2_PLACEMENT_3D('',#6847,#5114,#5115);
#4281=AXIS2_PLACEMENT_3D('',#6849,#5116,#5117);
#4282=AXIS2_PLACEMENT_3D('',#6852,#5119,#5120);
#4283=AXIS2_PLACEMENT_3D('',#6853,#5121,#5122);
#4284=AXIS2_PLACEMENT_3D('',#6855,#5123,#5124);
#4285=AXIS2_PLACEMENT_3D('',#6856,#5125,#5126);
#4286=AXIS2_PLACEMENT_3D('',#6858,#5127,#5128);
#4287=AXIS2_PLACEMENT_3D('',#6860,#5130,#5131);
#4288=AXIS2_PLACEMENT_3D('',#6862,#5132,#5133);
#4289=AXIS2_PLACEMENT_3D('',#6863,#5134,#5135);
#4290=AXIS2_PLACEMENT_3D('',#6865,#5136,#5137);
#4291=AXIS2_PLACEMENT_3D('',#6867,#5139,#5140);
#4292=AXIS2_PLACEMENT_3D('',#6869,#5142,#5143);
#4293=AXIS2_PLACEMENT_3D('',#6870,#5144,#5145);
#4294=AXIS2_PLACEMENT_3D('',#6923,#5149,#5150);
#4295=AXIS2_PLACEMENT_3D('',#6965,#5153,#5154);
#4296=AXIS2_PLACEMENT_3D('',#7007,#5157,#5158);
#4297=AXIS2_PLACEMENT_3D('',#7049,#5161,#5162);
#4298=AXIS2_PLACEMENT_3D('',#7091,#5165,#5166);
#4299=AXIS2_PLACEMENT_3D('',#7130,#5168,#5169);
#4300=AXIS2_PLACEMENT_3D('',#7132,#5170,#5171);
#4301=AXIS2_PLACEMENT_3D('',#7133,#5172,#5173);
#4302=AXIS2_PLACEMENT_3D('',#7135,#5174,#5175);
#4303=AXIS2_PLACEMENT_3D('',#7137,#5177,#5178);
#4304=AXIS2_PLACEMENT_3D('',#7139,#5179,#5180);
#4305=AXIS2_PLACEMENT_3D('',#7140,#5181,#5182);
#4306=AXIS2_PLACEMENT_3D('',#7141,#5183,#5184);
#4307=AXIS2_PLACEMENT_3D('',#7142,#5185,#5186);
#4308=AXIS2_PLACEMENT_3D('',#7143,#5187,#5188);
#4309=AXIS2_PLACEMENT_3D('',#7144,#5189,#5190);
#4310=AXIS2_PLACEMENT_3D('',#7145,#5191,#5192);
#4311=AXIS2_PLACEMENT_3D('',#7146,#5193,#5194);
#4312=AXIS2_PLACEMENT_3D('',#7147,#5195,#5196);
#4313=AXIS2_PLACEMENT_3D('',#7148,#5197,#5198);
#4314=AXIS2_PLACEMENT_3D('',#7149,#5199,#5200);
#4315=AXIS2_PLACEMENT_3D('',#7150,#5201,#5202);
#4316=AXIS2_PLACEMENT_3D('',#7151,#5203,#5204);
#4317=AXIS2_PLACEMENT_3D('',#7152,#5205,#5206);
#4318=AXIS2_PLACEMENT_3D('',#7154,#5207,#5208);
#4319=AXIS2_PLACEMENT_3D('',#7156,#5209,#5210);
#4320=AXIS2_PLACEMENT_3D('',#7157,#5211,#5212);
#4321=AXIS2_PLACEMENT_3D('',#7159,#5214,#5215);
#4322=AXIS2_PLACEMENT_3D('',#7161,#5216,#5217);
#4323=AXIS2_PLACEMENT_3D('',#7163,#5219,#5220);
#4324=AXIS2_PLACEMENT_3D('',#7165,#5221,#5222);
#4325=AXIS2_PLACEMENT_3D('',#7166,#5223,#5224);
#4326=AXIS2_PLACEMENT_3D('',#7168,#5226,#5227);
#4327=AXIS2_PLACEMENT_3D('',#7169,#5228,#5229);
#4328=AXIS2_PLACEMENT_3D('',#7287,#5233,#5234);
#4329=AXIS2_PLACEMENT_3D('',#7408,#5238,#5239);
#4330=AXIS2_PLACEMENT_3D('',#7409,#5240,#5241);
#4331=AXIS2_PLACEMENT_3D('',#7424,#5242,#5243);
#4332=AXIS2_PLACEMENT_3D('',#7437,#5244,#5245);
#4333=AXIS2_PLACEMENT_3D('',#7442,#5247,#5248);
#4334=AXIS2_PLACEMENT_3D('',#7459,#5250,#5251);
#4335=AXIS2_PLACEMENT_3D('',#7461,#5252,#5253);
#4336=AXIS2_PLACEMENT_3D('',#7474,#5254,#5255);
#4337=AXIS2_PLACEMENT_3D('',#7479,#5257,#5258);
#4338=AXIS2_PLACEMENT_3D('',#7496,#5260,#5261);
#4339=AXIS2_PLACEMENT_3D('',#7509,#5262,#5263);
#4340=AXIS2_PLACEMENT_3D('',#7514,#5265,#5266);
#4341=AXIS2_PLACEMENT_3D('',#7531,#5268,#5269);
#4342=AXIS2_PLACEMENT_3D('',#7533,#5270,#5271);
#4343=AXIS2_PLACEMENT_3D('',#7546,#5272,#5273);
#4344=AXIS2_PLACEMENT_3D('',#7547,#5274,#5275);
#4345=AXIS2_PLACEMENT_3D('',#7562,#5276,#5277);
#4346=AXIS2_PLACEMENT_3D('',#7575,#5278,#5279);
#4347=AXIS2_PLACEMENT_3D('',#7580,#5281,#5282);
#4348=AXIS2_PLACEMENT_3D('',#7597,#5284,#5285);
#4349=AXIS2_PLACEMENT_3D('',#7610,#5286,#5287);
#4350=AXIS2_PLACEMENT_3D('',#7725,#5290,#5291);
#4351=AXIS2_PLACEMENT_3D('',#7834,#5294,#5295);
#4352=AXIS2_PLACEMENT_3D('',#7943,#5297,#5298);
#4353=AXIS2_PLACEMENT_3D('',#8055,#5300,#5301);
#4354=AXIS2_PLACEMENT_3D('',#8173,#5304,#5305);
#4355=AXIS2_PLACEMENT_3D('',#8285,#5308,#5309);
#4356=AXIS2_PLACEMENT_3D('',#8286,#5310,#5311);
#4357=AXIS2_PLACEMENT_3D('',#8299,#5312,#5313);
#4358=AXIS2_PLACEMENT_3D('',#8354,#5314,#5315);
#4359=AXIS2_PLACEMENT_3D('',#8368,#5316,#5317);
#4360=AXIS2_PLACEMENT_3D('',#8436,#5318,#5319);
#4361=AXIS2_PLACEMENT_3D('',#8540,#5320,#5321);
#4362=AXIS2_PLACEMENT_3D('',#8747,#5322,#5323);
#4363=AXIS2_PLACEMENT_3D('',#8869,#5324,#5325);
#4364=AXIS2_PLACEMENT_3D('',#8870,#5326,#5327);
#4365=AXIS2_PLACEMENT_3D('',#8895,#5328,#5329);
#4366=AXIS2_PLACEMENT_3D('',#8896,#5330,#5331);
#4367=AXIS2_PLACEMENT_3D('',#8921,#5332,#5333);
#4368=AXIS2_PLACEMENT_3D('',#8923,#5334,#5335);
#4369=AXIS2_PLACEMENT_3D('',#8926,#5337,#5338);
#4370=AXIS2_PLACEMENT_3D('',#8928,#5339,#5340);
#4371=AXIS2_PLACEMENT_3D('',#8931,#5342,#5343);
#4372=AXIS2_PLACEMENT_3D('',#8932,#5344,#5345);
#4373=AXIS2_PLACEMENT_3D('',#8933,#5346,#5347);
#4374=AXIS2_PLACEMENT_3D('',#8934,#5348,#5349);
#4375=AXIS2_PLACEMENT_3D('',#8935,#5350,#5351);
#4376=AXIS2_PLACEMENT_3D('',#8936,#5352,#5353);
#4377=AXIS2_PLACEMENT_3D('',#8937,#5354,#5355);
#4378=AXIS2_PLACEMENT_3D('',#8938,#5356,#5357);
#4379=AXIS2_PLACEMENT_3D('',#8939,#5358,#5359);
#4380=AXIS2_PLACEMENT_3D('',#8940,#5360,#5361);
#4381=AXIS2_PLACEMENT_3D('',#8949,#5366,#5367);
#4382=AXIS2_PLACEMENT_3D('',#8958,#5372,#5373);
#4383=AXIS2_PLACEMENT_3D('',#8961,#5376,#5377);
#4384=AXIS2_PLACEMENT_3D('',#8963,#5379,#5380);
#4385=AXIS2_PLACEMENT_3D('',#8965,#5382,#5383);
#4386=AXIS2_PLACEMENT_3D('',#8966,#5384,#5385);
#4387=AXIS2_PLACEMENT_3D('',#8967,#5386,#5387);
#4388=AXIS2_PLACEMENT_3D('',#8968,#5388,#5389);
#4389=AXIS2_PLACEMENT_3D('',#8969,#5390,#5391);
#4390=AXIS2_PLACEMENT_3D('',#8970,#5392,#5393);
#4391=AXIS2_PLACEMENT_3D('',#8971,#5394,#5395);
#4392=AXIS2_PLACEMENT_3D('',#8972,#5396,#5397);
#4393=AXIS2_PLACEMENT_3D('',#8973,#5398,#5399);
#4394=AXIS2_PLACEMENT_3D('',#9394,#5400,#5401);
#4395=AXIS2_PLACEMENT_3D('',#9395,#5402,#5403);
#4396=AXIS2_PLACEMENT_3D('',#9416,#5406,#5407);
#4397=AXIS2_PLACEMENT_3D('',#9434,#5409,#5410);
#4398=AXIS2_PLACEMENT_3D('',#9452,#5412,#5413);
#4399=AXIS2_PLACEMENT_3D('',#9470,#5415,#5416);
#4400=AXIS2_PLACEMENT_3D('',#9488,#5418,#5419);
#4401=AXIS2_PLACEMENT_3D('',#9503,#5420,#5421);
#4402=AXIS2_PLACEMENT_3D('',#9504,#5422,#5423);
#4403=AXIS2_PLACEMENT_3D('',#9505,#5424,#5425);
#4404=AXIS2_PLACEMENT_3D('',#9506,#5426,#5427);
#4405=AXIS2_PLACEMENT_3D('',#9507,#5428,#5429);
#4406=AXIS2_PLACEMENT_3D('',#9508,#5430,#5431);
#4407=AXIS2_PLACEMENT_3D('',#9509,#5432,#5433);
#4408=AXIS2_PLACEMENT_3D('',#9511,#5434,#5435);
#4409=AXIS2_PLACEMENT_3D('',#9512,#5436,#5437);
#4410=AXIS2_PLACEMENT_3D('',#9513,#5438,#5439);
#4411=AXIS2_PLACEMENT_3D('',#9514,#5440,#5441);
#4412=AXIS2_PLACEMENT_3D('',#9515,#5442,#5443);
#4413=AXIS2_PLACEMENT_3D('',#9516,#5444,#5445);
#4414=AXIS2_PLACEMENT_3D('',#9517,#5446,#5447);
#4415=AXIS2_PLACEMENT_3D('',#9518,#5448,#5449);
#4416=AXIS2_PLACEMENT_3D('',#9520,#5450,#5451);
#4417=AXIS2_PLACEMENT_3D('',#9521,#5452,#5453);
#4418=AXIS2_PLACEMENT_3D('',#9523,#5455,#5456);
#4419=AXIS2_PLACEMENT_3D('',#9524,#5457,#5458);
#4420=AXIS2_PLACEMENT_3D('',#9525,#5459,#5460);
#4421=AXIS2_PLACEMENT_3D('',#9526,#5461,#5462);
#4422=AXIS2_PLACEMENT_3D('',#9527,#5463,#5464);
#4423=AXIS2_PLACEMENT_3D('',#9528,#5465,#5466);
#4424=AXIS2_PLACEMENT_3D('',#9529,#5467,#5468);
#4425=AXIS2_PLACEMENT_3D('',#9530,#5469,#5470);
#4426=AXIS2_PLACEMENT_3D('',#9531,#5471,#5472);
#4427=AXIS2_PLACEMENT_3D('',#9532,#5473,#5474);
#4428=AXIS2_PLACEMENT_3D('',#9533,#5475,#5476);
#4429=AXIS2_PLACEMENT_3D('',#9534,#5477,#5478);
#4430=AXIS2_PLACEMENT_3D('',#9535,#5479,#5480);
#4431=AXIS2_PLACEMENT_3D('',#9536,#5481,#5482);
#4432=AXIS2_PLACEMENT_3D('',#9551,#5486,#5487);
#4433=AXIS2_PLACEMENT_3D('',#9563,#5490,#5491);
#4434=AXIS2_PLACEMENT_3D('',#9575,#5494,#5495);
#4435=AXIS2_PLACEMENT_3D('',#9587,#5498,#5499);
#4436=AXIS2_PLACEMENT_3D('',#9599,#5502,#5503);
#4437=AXIS2_PLACEMENT_3D('',#9608,#5505,#5506);
#4438=AXIS2_PLACEMENT_3D('',#9610,#5507,#5508);
#4439=AXIS2_PLACEMENT_3D('',#9613,#5510,#5511);
#4440=AXIS2_PLACEMENT_3D('',#9614,#5512,#5513);
#4441=AXIS2_PLACEMENT_3D('',#9615,#5514,#5515);
#4442=AXIS2_PLACEMENT_3D('',#9616,#5516,#5517);
#4443=AXIS2_PLACEMENT_3D('',#9617,#5518,#5519);
#4444=AXIS2_PLACEMENT_3D('',#9618,#5520,#5521);
#4445=AXIS2_PLACEMENT_3D('',#9619,#5522,#5523);
#4446=AXIS2_PLACEMENT_3D('',#9620,#5524,#5525);
#4447=AXIS2_PLACEMENT_3D('',#9621,#5526,#5527);
#4448=AXIS2_PLACEMENT_3D('',#9622,#5528,#5529);
#4449=AXIS2_PLACEMENT_3D('',#9623,#5530,#5531);
#4450=AXIS2_PLACEMENT_3D('',#9624,#5532,#5533);
#4451=AXIS2_PLACEMENT_3D('',#9625,#5534,#5535);
#4452=AXIS2_PLACEMENT_3D('',#9626,#5536,#5537);
#4453=AXIS2_PLACEMENT_3D('',#9627,#5538,#5539);
#4454=AXIS2_PLACEMENT_3D('',#9628,#5540,#5541);
#4455=AXIS2_PLACEMENT_3D('',#9629,#5542,#5543);
#4456=AXIS2_PLACEMENT_3D('',#9630,#5544,#5545);
#4457=AXIS2_PLACEMENT_3D('',#9631,#5546,#5547);
#4458=AXIS2_PLACEMENT_3D('',#9632,#5548,#5549);
#4459=AXIS2_PLACEMENT_3D('',#9633,#5550,#5551);
#4460=AXIS2_PLACEMENT_3D('',#9634,#5552,#5553);
#4461=AXIS2_PLACEMENT_3D('',#9635,#5554,#5555);
#4462=AXIS2_PLACEMENT_3D('',#9636,#5556,#5557);
#4463=AXIS2_PLACEMENT_3D('',#9637,#5558,#5559);
#4464=AXIS2_PLACEMENT_3D('',#9638,#5560,#5561);
#4465=AXIS2_PLACEMENT_3D('',#9639,#5562,#5563);
#4466=AXIS2_PLACEMENT_3D('',#9640,#5564,#5565);
#4467=AXIS2_PLACEMENT_3D('',#9641,#5566,#5567);
#4468=AXIS2_PLACEMENT_3D('',#9642,#5568,#5569);
#4469=DIRECTION('axis',(0.,0.,1.));
#4470=DIRECTION('refdir',(1.,0.,0.));
#4471=DIRECTION('axis',(0.,0.,1.));
#4472=DIRECTION('refdir',(1.,0.,0.));
#4473=DIRECTION('center_axis',(3.43024899888577E-15,-1.,0.));
#4474=DIRECTION('ref_axis',(-1.,-3.31586610021379E-15,-6.12323399573677E-17));
#4475=DIRECTION('center_axis',(3.43024899888577E-15,-1.,0.));
#4476=DIRECTION('ref_axis',(1.,3.43024899888577E-15,0.));
#4477=DIRECTION('center_axis',(3.43024899888577E-15,-1.,0.));
#4478=DIRECTION('ref_axis',(1.,3.43024899888577E-15,0.));
#4479=DIRECTION('center_axis',(3.43024899888577E-15,-1.,0.));
#4480=DIRECTION('ref_axis',(1.,3.43024899888577E-15,0.));
#4481=DIRECTION('center_axis',(1.,0.,0.));
#4482=DIRECTION('ref_axis',(0.,0.,-1.));
#4483=DIRECTION('',(1.,3.39178734177461E-15,0.));
#4484=DIRECTION('',(-1.,0.,0.));
#4485=DIRECTION('center_axis',(1.,0.,0.));
#4486=DIRECTION('ref_axis',(0.,0.,-1.));
#4487=DIRECTION('',(-1.,-3.39178430813906E-15,0.));
#4488=DIRECTION('center_axis',(3.43024899888577E-15,-1.,0.));
#4489=DIRECTION('ref_axis',(0.,0.,-1.));
#4490=DIRECTION('center_axis',(3.43024899888577E-15,-1.,0.));
#4491=DIRECTION('ref_axis',(1.,3.43024899888577E-15,0.));
#4492=DIRECTION('center_axis',(3.43024899888577E-15,-1.,0.));
#4493=DIRECTION('ref_axis',(1.,3.43024899888577E-15,0.));
#4494=DIRECTION('center_axis',(1.,3.43024899888577E-15,1.22464679914735E-16));
#4495=DIRECTION('ref_axis',(-1.22464679914735E-16,0.,1.));
#4496=DIRECTION('center_axis',(3.43024899888577E-15,-1.,0.));
#4497=DIRECTION('ref_axis',(1.,3.43024899888577E-15,0.));
#4498=DIRECTION('center_axis',(3.43024899888577E-15,-1.,0.));
#4499=DIRECTION('ref_axis',(1.,3.43024899888577E-15,0.));
#4500=DIRECTION('center_axis',(3.43024899888577E-15,-1.,0.));
#4501=DIRECTION('ref_axis',(0.,0.,-1.));
#4502=DIRECTION('center_axis',(3.43024899888577E-15,-1.,0.));
#4503=DIRECTION('ref_axis',(1.,3.43024899888577E-15,0.));
#4504=DIRECTION('',(1.,3.40592503341502E-15,0.));
#4505=DIRECTION('',(-1.,-3.40592503341502E-15,0.));
#4506=DIRECTION('center_axis',(3.43024899888577E-15,-1.,0.));
#4507=DIRECTION('ref_axis',(1.,3.43024899888577E-15,0.));
#4508=DIRECTION('center_axis',(3.43024899888577E-15,-1.,0.));
#4509=DIRECTION('ref_axis',(1.,3.43024899888577E-15,0.));
#4510=DIRECTION('center_axis',(3.43024899888577E-15,-1.,0.));
#4511=DIRECTION('ref_axis',(1.,3.43024899888577E-15,0.));
#4512=DIRECTION('center_axis',(3.43024899888577E-15,-1.,0.));
#4513=DIRECTION('ref_axis',(1.,3.43024899888577E-15,0.));
#4514=DIRECTION('center_axis',(-3.43024899888577E-15,1.,0.));
#4515=DIRECTION('ref_axis',(0.,0.,1.));
#4516=DIRECTION('center_axis',(3.43024899888577E-15,-1.,0.));
#4517=DIRECTION('ref_axis',(1.,3.43024899888577E-15,0.));
#4518=DIRECTION('center_axis',(3.43024899888577E-15,-1.,0.));
#4519=DIRECTION('ref_axis',(1.,3.43024899888577E-15,0.));
#4520=DIRECTION('center_axis',(-3.43024899888577E-15,1.,0.));
#4521=DIRECTION('ref_axis',(-1.,-3.43024899888577E-15,0.));
#4522=DIRECTION('center_axis',(3.43024899888577E-15,-1.,0.));
#4523=DIRECTION('ref_axis',(1.,3.43024899888577E-15,0.));
#4524=DIRECTION('center_axis',(3.43024899888577E-15,-1.,0.));
#4525=DIRECTION('ref_axis',(1.,3.43024899888577E-15,0.));
#4526=DIRECTION('',(0.707106781186544,0.707106781186551,-8.65956056235492E-17));
#4527=DIRECTION('center_axis',(3.43024899888577E-15,-1.,0.));
#4528=DIRECTION('ref_axis',(1.,3.43024899888577E-15,0.));
#4529=DIRECTION('',(3.43024899888577E-15,-1.,0.));
#4530=DIRECTION('center_axis',(3.43024899888577E-15,-1.,0.));
#4531=DIRECTION('ref_axis',(1.,3.43024899888577E-15,0.));
#4532=DIRECTION('center_axis',(-3.43024899888577E-15,1.,0.));
#4533=DIRECTION('ref_axis',(0.,0.,1.));
#4534=DIRECTION('center_axis',(3.43024899888577E-15,-1.,0.));
#4535=DIRECTION('ref_axis',(1.,3.43024899888577E-15,0.));
#4536=DIRECTION('center_axis',(3.43024899888577E-15,-1.,0.));
#4537=DIRECTION('ref_axis',(1.,3.43024899888577E-15,0.));
#4538=DIRECTION('',(3.43024899888577E-15,-1.,0.));
#4539=DIRECTION('center_axis',(3.43024899888577E-15,-1.,0.));
#4540=DIRECTION('ref_axis',(1.,3.43024899888577E-15,0.));
#4541=DIRECTION('center_axis',(3.43024899888577E-15,-1.,0.));
#4542=DIRECTION('ref_axis',(0.,0.,-1.));
#4543=DIRECTION('center_axis',(3.43024899888577E-15,-1.,0.));
#4544=DIRECTION('ref_axis',(1.,3.43024899888577E-15,0.));
#4545=DIRECTION('center_axis',(3.43024899888577E-15,-1.,0.));
#4546=DIRECTION('ref_axis',(-3.49148133884313E-15,-1.22273440309257E-29,
-1.));
#4547=DIRECTION('center_axis',(3.43024899888577E-15,-1.,0.));
#4548=DIRECTION('ref_axis',(-1.,-3.43024899888577E-15,0.));
#4549=DIRECTION('center_axis',(3.43024899888577E-15,-1.,0.));
#4550=DIRECTION('ref_axis',(1.04744440165294E-14,3.5893171187556E-29,1.));
#4551=DIRECTION('center_axis',(3.43024899888577E-15,-1.,0.));
#4552=DIRECTION('ref_axis',(1.,3.43024899888577E-15,0.));
#4553=DIRECTION('center_axis',(3.43024899888577E-15,-1.,0.));
#4554=DIRECTION('ref_axis',(1.,3.43024899888577E-15,0.));
#4555=DIRECTION('',(-3.43024899888577E-15,1.,0.));
#4556=DIRECTION('center_axis',(-3.43024899888577E-15,1.,0.));
#4557=DIRECTION('ref_axis',(-1.,-3.43024899888577E-15,0.));
#4558=DIRECTION('center_axis',(-3.43024899888577E-15,1.,0.));
#4559=DIRECTION('ref_axis',(-1.,-3.43024899888577E-15,0.));
#4560=DIRECTION('center_axis',(-3.43024899888577E-15,1.,0.));
#4561=DIRECTION('ref_axis',(0.,0.,1.));
#4562=DIRECTION('center_axis',(-3.43024899888577E-15,1.,0.));
#4563=DIRECTION('ref_axis',(-1.,-3.43024899888577E-15,0.));
#4564=DIRECTION('center_axis',(-3.43024899888577E-15,1.,0.));
#4565=DIRECTION('ref_axis',(-1.,-3.43024899888577E-15,0.));
#4566=DIRECTION('center_axis',(-3.43024899888577E-15,1.,0.));
#4567=DIRECTION('ref_axis',(-1.,-3.43024899888577E-15,0.));
#4568=DIRECTION('center_axis',(-3.43024899888577E-15,1.,0.));
#4569=DIRECTION('ref_axis',(-1.,-3.43024899888577E-15,0.));
#4570=DIRECTION('center_axis',(-3.43024899888577E-15,1.,0.));
#4571=DIRECTION('ref_axis',(-1.,-3.43024899888577E-15,0.));
#4572=DIRECTION('center_axis',(3.43024899888577E-15,-1.,0.));
#4573=DIRECTION('ref_axis',(1.,3.43024899888577E-15,0.));
#4574=DIRECTION('center_axis',(3.43024899888577E-15,-1.,0.));
#4575=DIRECTION('ref_axis',(1.,3.43024899888577E-15,0.));
#4576=DIRECTION('',(-3.43024899888577E-15,1.,0.));
#4577=DIRECTION('center_axis',(3.43024899888577E-15,-1.,0.));
#4578=DIRECTION('ref_axis',(1.,3.43024899888577E-15,0.));
#4579=DIRECTION('center_axis',(3.43024899888577E-15,-1.,0.));
#4580=DIRECTION('ref_axis',(1.,3.43024899888577E-15,0.));
#4581=DIRECTION('center_axis',(3.43024899888577E-15,-1.,0.));
#4582=DIRECTION('ref_axis',(0.,0.,-1.));
#4583=DIRECTION('center_axis',(1.,3.43024899888577E-15,1.22464679914735E-16));
#4584=DIRECTION('ref_axis',(-1.22464679914735E-16,0.,1.));
#4585=DIRECTION('center_axis',(3.43024899888577E-15,-1.,0.));
#4586=DIRECTION('ref_axis',(1.,3.43024899888577E-15,0.));
#4587=DIRECTION('center_axis',(3.43024899888577E-15,-1.,0.));
#4588=DIRECTION('ref_axis',(0.,0.,-1.));
#4589=DIRECTION('center_axis',(3.43024899888577E-15,-1.,0.));
#4590=DIRECTION('ref_axis',(1.,3.43024899888577E-15,0.));
#4591=DIRECTION('center_axis',(3.43024899888577E-15,-1.,0.));
#4592=DIRECTION('ref_axis',(0.,0.,-1.));
#4593=DIRECTION('center_axis',(-1.,-3.43024899888577E-15,-1.22464679914735E-16));
#4594=DIRECTION('ref_axis',(-1.22464679914735E-16,0.,1.));
#4595=DIRECTION('center_axis',(3.43024899888577E-15,-1.,0.));
#4596=DIRECTION('ref_axis',(1.,3.43024899888577E-15,0.));
#4597=DIRECTION('center_axis',(3.43024899888577E-15,-1.,0.));
#4598=DIRECTION('ref_axis',(1.,3.43024899888577E-15,0.));
#4599=DIRECTION('center_axis',(3.43024899888577E-15,-1.,0.));
#4600=DIRECTION('ref_axis',(1.,3.43024899888577E-15,0.));
#4601=DIRECTION('center_axis',(3.43024899888577E-15,-1.,0.));
#4602=DIRECTION('ref_axis',(1.,3.43024899888577E-15,0.));
#4603=DIRECTION('',(-3.43024899888577E-15,1.,0.));
#4604=DIRECTION('center_axis',(3.43024899888577E-15,-1.,0.));
#4605=DIRECTION('ref_axis',(1.,3.43024899888577E-15,0.));
#4606=DIRECTION('',(2.23596159769488E-15,-1.,0.));
#4607=DIRECTION('',(-3.43024899888577E-15,1.,0.));
#4608=DIRECTION('center_axis',(3.43024899888577E-15,-1.,0.));
#4609=DIRECTION('ref_axis',(1.,3.43024899888577E-15,0.));
#4610=DIRECTION('',(2.23596159769488E-15,-1.,0.));
#4611=DIRECTION('center_axis',(-3.43024899888577E-15,1.,0.));
#4612=DIRECTION('ref_axis',(0.,0.,1.));
#4613=DIRECTION('center_axis',(-3.43024899888577E-15,1.,0.));
#4614=DIRECTION('ref_axis',(-1.,-3.43024899888577E-15,0.));
#4615=DIRECTION('center_axis',(3.43024899888572E-15,-1.,-3.43024899888575E-15));
#4616=DIRECTION('ref_axis',(1.,3.43024899888575E-15,-1.04744440165294E-14));
#4617=DIRECTION('center_axis',(6.86049799777151E-15,-1.,0.));
#4618=DIRECTION('ref_axis',(0.,0.,1.));
#4619=DIRECTION('center_axis',(3.43024899888577E-15,-1.,3.43024899888575E-15));
#4620=DIRECTION('ref_axis',(-1.,-3.43024899888575E-15,3.49148133884313E-15));
#4621=DIRECTION('center_axis',(0.,-1.,0.));
#4622=DIRECTION('ref_axis',(0.,0.,-1.));
#4623=DIRECTION('center_axis',(3.43024899888577E-15,-1.,0.));
#4624=DIRECTION('ref_axis',(1.,3.43024899888577E-15,0.));
#4625=DIRECTION('center_axis',(-3.43024899888577E-15,1.,0.));
#4626=DIRECTION('ref_axis',(-1.,-3.43024899888577E-15,0.));
#4627=DIRECTION('center_axis',(-3.43024899888577E-15,1.,0.));
#4628=DIRECTION('ref_axis',(-1.,-3.43024899888577E-15,0.));
#4629=DIRECTION('',(3.43024899888577E-15,-1.,0.));
#4630=DIRECTION('center_axis',(3.43024899888577E-15,-1.,0.));
#4631=DIRECTION('ref_axis',(1.,3.43024899888577E-15,0.));
#4632=DIRECTION('center_axis',(3.43024899888577E-15,-1.,0.));
#4633=DIRECTION('ref_axis',(0.,0.,-1.));
#4634=DIRECTION('center_axis',(3.43024899888577E-15,-1.,0.));
#4635=DIRECTION('ref_axis',(1.,3.43024899888577E-15,0.));
#4636=DIRECTION('center_axis',(3.43024899888577E-15,-1.,0.));
#4637=DIRECTION('ref_axis',(1.,3.43024899888577E-15,0.));
#4638=DIRECTION('',(3.43024899888577E-15,-1.,0.));
#4639=DIRECTION('center_axis',(3.43024899888577E-15,-1.,0.));
#4640=DIRECTION('ref_axis',(1.,3.43024899888577E-15,0.));
#4641=DIRECTION('center_axis',(-3.43024899888577E-15,1.,0.));
#4642=DIRECTION('ref_axis',(0.,0.,1.));
#4643=DIRECTION('center_axis',(3.43024899888577E-15,-1.,0.));
#4644=DIRECTION('ref_axis',(1.,3.43024899888577E-15,0.));
#4645=DIRECTION('center_axis',(3.43024899888577E-15,-1.,0.));
#4646=DIRECTION('ref_axis',(0.,0.,-1.));
#4647=DIRECTION('center_axis',(1.,3.43024899888577E-15,1.22464679914735E-16));
#4648=DIRECTION('ref_axis',(-1.22464679914735E-16,-3.84810197668786E-31,
1.));
#4649=DIRECTION('center_axis',(1.,0.,0.));
#4650=DIRECTION('ref_axis',(0.,0.,-1.));
#4651=DIRECTION('center_axis',(1.,0.,0.));
#4652=DIRECTION('ref_axis',(0.,0.,-1.));
#4653=DIRECTION('',(-1.,0.,0.));
#4654=DIRECTION('center_axis',(1.,0.,0.));
#4655=DIRECTION('ref_axis',(0.,0.,-1.));
#4656=DIRECTION('center_axis',(1.,0.,0.));
#4657=DIRECTION('ref_axis',(0.,0.,-1.));
#4658=DIRECTION('center_axis',(1.,0.,0.));
#4659=DIRECTION('ref_axis',(0.,0.,-1.));
#4660=DIRECTION('center_axis',(1.,0.,0.));
#4661=DIRECTION('ref_axis',(0.,0.,-1.));
#4662=DIRECTION('center_axis',(1.,0.,0.));
#4663=DIRECTION('ref_axis',(0.,0.,-1.));
#4664=DIRECTION('center_axis',(1.,0.,0.));
#4665=DIRECTION('ref_axis',(0.,0.,-1.));
#4666=DIRECTION('center_axis',(1.,0.,0.));
#4667=DIRECTION('ref_axis',(0.,0.,-1.));
#4668=DIRECTION('center_axis',(1.,0.,0.));
#4669=DIRECTION('ref_axis',(0.,-1.,3.49148133884313E-15));
#4670=DIRECTION('center_axis',(1.,0.,0.));
#4671=DIRECTION('ref_axis',(0.,0.,1.));
#4672=DIRECTION('center_axis',(1.,0.,0.));
#4673=DIRECTION('ref_axis',(0.,1.,-1.04744440165294E-14));
#4674=DIRECTION('center_axis',(1.,0.,0.));
#4675=DIRECTION('ref_axis',(0.,0.,-1.));
#4676=DIRECTION('center_axis',(1.,0.,0.));
#4677=DIRECTION('ref_axis',(0.,0.,-1.));
#4678=DIRECTION('center_axis',(-3.43024899888577E-15,1.,0.));
#4679=DIRECTION('ref_axis',(0.999999999999977,3.43024899888569E-15,2.15720406748434E-7));
#4680=DIRECTION('',(-3.55190708269137E-15,1.,0.));
#4681=DIRECTION('',(-3.32971747973986E-15,1.,0.));
#4682=DIRECTION('center_axis',(0.,0.,1.));
#4683=DIRECTION('ref_axis',(1.,0.,0.));
#4684=DIRECTION('',(-3.38353683695286E-15,1.,0.));
#4685=DIRECTION('center_axis',(0.,0.,-1.));
#4686=DIRECTION('ref_axis',(-1.,0.,0.));
#4687=DIRECTION('',(-3.38353683695286E-15,1.,0.));
#4688=DIRECTION('center_axis',(1.,0.,0.));
#4689=DIRECTION('ref_axis',(0.,0.,-1.));
#4690=DIRECTION('',(1.,0.,0.));
#4691=DIRECTION('center_axis',(1.,0.,0.));
#4692=DIRECTION('ref_axis',(0.,0.,-1.));
#4693=DIRECTION('',(1.,0.,0.));
#4694=DIRECTION('center_axis',(1.,0.,0.));
#4695=DIRECTION('ref_axis',(0.,0.,-1.));
#4696=DIRECTION('',(1.,0.,0.));
#4697=DIRECTION('center_axis',(1.,0.,0.));
#4698=DIRECTION('ref_axis',(0.,0.,-1.));
#4699=DIRECTION('',(1.,0.,0.));
#4700=DIRECTION('center_axis',(1.,0.,0.));
#4701=DIRECTION('ref_axis',(0.,0.,-1.));
#4702=DIRECTION('',(1.,0.,0.));
#4703=DIRECTION('center_axis',(3.43024899888577E-15,-1.,0.));
#4704=DIRECTION('ref_axis',(1.,3.43024899888577E-15,0.));
#4705=DIRECTION('',(3.43024899888577E-15,-1.,0.));
#4706=DIRECTION('center_axis',(3.43024899888577E-15,-1.,0.));
#4707=DIRECTION('ref_axis',(1.,3.43024899888577E-15,0.));
#4708=DIRECTION('',(3.43024899888577E-15,-1.,0.));
#4709=DIRECTION('center_axis',(3.43024899888577E-15,-1.,0.));
#4710=DIRECTION('ref_axis',(1.,3.43024899888577E-15,0.));
#4711=DIRECTION('',(3.43024899888577E-15,-1.,0.));
#4712=DIRECTION('center_axis',(3.43024899888577E-15,-1.,0.));
#4713=DIRECTION('ref_axis',(1.,3.43024899888577E-15,0.));
#4714=DIRECTION('',(3.43024899888577E-15,-1.,0.));
#4715=DIRECTION('center_axis',(0.,-1.,0.));
#4716=DIRECTION('ref_axis',(0.,0.,-1.));
#4717=DIRECTION('',(0.,-1.,0.));
#4718=DIRECTION('center_axis',(0.,-1.,0.));
#4719=DIRECTION('ref_axis',(0.,0.,-1.));
#4720=DIRECTION('center_axis',(0.,-1.,0.));
#4721=DIRECTION('ref_axis',(0.,0.,-1.));
#4722=DIRECTION('center_axis',(0.,1.,0.));
#4723=DIRECTION('ref_axis',(0.,0.,1.));
#4724=DIRECTION('',(-1.04972719113862E-16,0.515038074910052,-0.857167300702114));
#4725=DIRECTION('center_axis',(3.43024899888577E-15,-1.,3.43024899888575E-15));
#4726=DIRECTION('ref_axis',(-1.,-3.43024899888575E-15,3.49148133884313E-15));
#4727=DIRECTION('',(3.43024899888577E-15,-1.,3.43024899888575E-15));
#4728=DIRECTION('center_axis',(6.86049799777151E-15,-1.,0.));
#4729=DIRECTION('ref_axis',(0.,0.,1.));
#4730=DIRECTION('',(6.86049799777151E-15,-1.,0.));
#4731=DIRECTION('center_axis',(3.43024899888572E-15,-1.,-3.43024899888575E-15));
#4732=DIRECTION('ref_axis',(1.,3.43024899888575E-15,-1.04744440165294E-14));
#4733=DIRECTION('',(3.43024899888572E-15,-1.,-3.43024899888575E-15));
#4734=DIRECTION('center_axis',(3.43024899888577E-15,-1.,0.));
#4735=DIRECTION('ref_axis',(1.,3.43024899888577E-15,0.));
#4736=DIRECTION('center_axis',(3.43024899888577E-15,-1.,0.));
#4737=DIRECTION('ref_axis',(1.,3.43024899888577E-15,0.));
#4738=DIRECTION('center_axis',(-3.43024899888577E-15,1.,0.));
#4739=DIRECTION('ref_axis',(0.,0.,1.));
#4740=DIRECTION('center_axis',(-1.,-3.43024899888577E-15,1.22464679914735E-16));
#4741=DIRECTION('ref_axis',(-1.22464679914735E-16,0.,-1.));
#4742=DIRECTION('center_axis',(-3.43024899888577E-15,1.,0.));
#4743=DIRECTION('ref_axis',(0.,0.,1.));
#4744=DIRECTION('center_axis',(-1.,-3.43024899888577E-15,1.22464679914735E-16));
#4745=DIRECTION('ref_axis',(-1.22464679914735E-16,0.,-1.));
#4746=DIRECTION('axis',(0.,0.,1.));
#4747=DIRECTION('refdir',(1.,0.,0.));
#4748=DIRECTION('center_axis',(0.,-1.,0.));
#4749=DIRECTION('ref_axis',(0.,0.,-1.));
#4750=DIRECTION('center_axis',(0.,-1.,0.));
#4751=DIRECTION('ref_axis',(0.,0.,-1.));
#4752=DIRECTION('',(3.50382346376903E-15,0.,-1.));
#4753=DIRECTION('',(1.,0.,0.));
#4754=DIRECTION('center_axis',(0.,-1.,0.));
#4755=DIRECTION('ref_axis',(0.,0.,-1.));
#4756=DIRECTION('',(1.,0.,0.));
#4757=DIRECTION('',(-3.49222139931946E-15,0.,1.));
#4758=DIRECTION('center_axis',(0.,-1.,0.));
#4759=DIRECTION('ref_axis',(0.,0.,-1.));
#4760=DIRECTION('center_axis',(0.,-1.,0.));
#4761=DIRECTION('ref_axis',(0.,0.,-1.));
#4762=DIRECTION('',(-1.,0.,0.));
#4763=DIRECTION('',(3.4806193348699E-15,0.,-1.));
#4764=DIRECTION('center_axis',(0.,-1.,0.));
#4765=DIRECTION('ref_axis',(0.,0.,-1.));
#4766=DIRECTION('center_axis',(0.,-1.,0.));
#4767=DIRECTION('ref_axis',(0.,0.,-1.));
#4768=DIRECTION('center_axis',(0.,-1.,0.));
#4769=DIRECTION('ref_axis',(0.,0.,-1.));
#4770=DIRECTION('',(-3.4806193348699E-15,0.,1.));
#4771=DIRECTION('',(-1.,0.,0.));
#4772=DIRECTION('center_axis',(0.,0.,-1.));
#4773=DIRECTION('ref_axis',(-1.,0.,0.));
#4774=DIRECTION('',(0.,1.,0.));
#4775=DIRECTION('',(-1.,0.,0.));
#4776=DIRECTION('',(0.,-1.,0.));
#4777=DIRECTION('center_axis',(0.,0.,-1.));
#4778=DIRECTION('ref_axis',(-1.,0.,0.));
#4779=DIRECTION('',(-1.,0.,0.));
#4780=DIRECTION('',(0.,1.,0.));
#4781=DIRECTION('',(0.,1.,0.));
#4782=DIRECTION('center_axis',(0.,0.,1.));
#4783=DIRECTION('ref_axis',(1.,0.,0.));
#4784=DIRECTION('',(1.,0.,0.));
#4785=DIRECTION('',(0.,1.,0.));
#4786=DIRECTION('',(0.,1.,0.));
#4787=DIRECTION('center_axis',(0.,0.,1.));
#4788=DIRECTION('ref_axis',(1.,0.,0.));
#4789=DIRECTION('',(0.,1.,0.));
#4790=DIRECTION('',(1.,0.,0.));
#4791=DIRECTION('',(0.,-1.,0.));
#4792=DIRECTION('center_axis',(0.,1.,0.));
#4793=DIRECTION('ref_axis',(0.,0.,1.));
#4794=DIRECTION('center_axis',(0.,-1.,0.));
#4795=DIRECTION('ref_axis',(0.,0.,-1.));
#4796=DIRECTION('center_axis',(0.,1.,0.));
#4797=DIRECTION('ref_axis',(0.,0.,1.));
#4798=DIRECTION('center_axis',(0.,-1.,0.));
#4799=DIRECTION('ref_axis',(0.,0.,-1.));
#4800=DIRECTION('',(0.,-1.,0.));
#4801=DIRECTION('center_axis',(0.,1.,0.));
#4802=DIRECTION('ref_axis',(0.,0.,1.));
#4803=DIRECTION('',(0.,1.,0.));
#4804=DIRECTION('center_axis',(0.,1.,0.));
#4805=DIRECTION('ref_axis',(0.,0.,1.));
#4806=DIRECTION('',(0.,-1.,0.));
#4807=DIRECTION('center_axis',(0.,-1.,0.));
#4808=DIRECTION('ref_axis',(0.,0.,-1.));
#4809=DIRECTION('',(0.,-1.,0.));
#4810=DIRECTION('center_axis',(0.,1.,0.));
#4811=DIRECTION('ref_axis',(0.,0.,1.));
#4812=DIRECTION('',(0.,-1.,0.));
#4813=DIRECTION('center_axis',(0.,-1.,0.));
#4814=DIRECTION('ref_axis',(0.,0.,-1.));
#4815=DIRECTION('center_axis',(0.,1.,0.));
#4816=DIRECTION('ref_axis',(0.,0.,1.));
#4817=DIRECTION('center_axis',(0.,-1.,0.));
#4818=DIRECTION('ref_axis',(0.,0.,-1.));
#4819=DIRECTION('',(0.,0.,1.));
#4820=DIRECTION('',(0.,0.,1.));
#4821=DIRECTION('center_axis',(0.,-1.,0.));
#4822=DIRECTION('ref_axis',(0.,0.,-1.));
#4823=DIRECTION('center_axis',(0.,-1.,0.));
#4824=DIRECTION('ref_axis',(0.,0.,-1.));
#4825=DIRECTION('center_axis',(0.,-1.,0.));
#4826=DIRECTION('ref_axis',(0.,0.,-1.));
#4827=DIRECTION('',(0.,1.,0.));
#4828=DIRECTION('center_axis',(0.,1.,0.));
#4829=DIRECTION('ref_axis',(0.,0.,1.));
#4830=DIRECTION('',(8.65956056235493E-17,-0.707106781186548,0.707106781186547));
#4831=DIRECTION('center_axis',(0.,-1.,0.));
#4832=DIRECTION('ref_axis',(1.,0.,3.49148133884313E-15));
#4833=DIRECTION('center_axis',(0.,-1.,0.));
#4834=DIRECTION('ref_axis',(0.,0.,-1.));
#4835=DIRECTION('center_axis',(0.,-1.,0.));
#4836=DIRECTION('ref_axis',(1.,0.,3.49148133884313E-15));
#4837=DIRECTION('center_axis',(0.,-1.,0.));
#4838=DIRECTION('ref_axis',(0.,0.,-1.));
#4839=DIRECTION('center_axis',(0.,-1.,0.));
#4840=DIRECTION('ref_axis',(1.,0.,3.49148133884313E-15));
#4841=DIRECTION('center_axis',(-1.,0.,0.));
#4842=DIRECTION('ref_axis',(0.,0.,1.));
#4843=DIRECTION('',(0.,0.,1.));
#4844=DIRECTION('center_axis',(0.,1.,0.));
#4845=DIRECTION('ref_axis',(0.,0.,1.));
#4846=DIRECTION('',(0.,0.,1.));
#4847=DIRECTION('center_axis',(0.,1.,0.));
#4848=DIRECTION('ref_axis',(0.,0.,1.));
#4849=DIRECTION('center_axis',(1.,0.,0.));
#4850=DIRECTION('ref_axis',(0.,0.,-1.));
#4851=DIRECTION('center_axis',(0.,-1.,0.));
#4852=DIRECTION('ref_axis',(0.,0.,-1.));
#4853=DIRECTION('',(0.,-1.,0.));
#4854=DIRECTION('center_axis',(0.,1.,0.));
#4855=DIRECTION('ref_axis',(0.,0.,1.));
#4856=DIRECTION('center_axis',(0.,-1.,0.));
#4857=DIRECTION('ref_axis',(0.,0.,-1.));
#4858=DIRECTION('center_axis',(0.,1.,0.));
#4859=DIRECTION('ref_axis',(0.,0.,1.));
#4860=DIRECTION('center_axis',(0.,-1.,0.));
#4861=DIRECTION('ref_axis',(0.,0.,-1.));
#4862=DIRECTION('center_axis',(0.,-1.,0.));
#4863=DIRECTION('ref_axis',(0.,0.,-1.));
#4864=DIRECTION('',(-3.48532219369785E-15,0.,1.));
#4865=DIRECTION('center_axis',(0.,-1.,0.));
#4866=DIRECTION('ref_axis',(0.,0.,-1.));
#4867=DIRECTION('',(3.48532219369785E-15,0.,-1.));
#4868=DIRECTION('center_axis',(0.,-1.,0.));
#4869=DIRECTION('ref_axis',(0.,0.,-1.));
#4870=DIRECTION('',(3.51320477124743E-15,0.,-1.));
#4871=DIRECTION('center_axis',(0.,-1.,0.));
#4872=DIRECTION('ref_axis',(0.,0.,-1.));
#4873=DIRECTION('',(-3.49926348247264E-15,0.,1.));
#4874=DIRECTION('center_axis',(0.,-1.,0.));
#4875=DIRECTION('ref_axis',(0.,0.,-1.));
#4876=DIRECTION('center_axis',(-1.,0.,-3.49148133884313E-15));
#4877=DIRECTION('ref_axis',(-3.49148133884313E-15,0.,1.));
#4878=DIRECTION('',(0.,1.,0.));
#4879=DIRECTION('center_axis',(1.,0.,3.49148133884313E-15));
#4880=DIRECTION('ref_axis',(3.49148133884313E-15,0.,-1.));
#4881=DIRECTION('',(0.,1.,0.));
#4882=DIRECTION('center_axis',(0.,1.,0.));
#4883=DIRECTION('ref_axis',(3.67517835871524E-15,0.,-1.));
#4884=DIRECTION('center_axis',(0.,-1.,0.));
#4885=DIRECTION('ref_axis',(0.,0.,-1.));
#4886=DIRECTION('center_axis',(1.,0.,3.49148133884313E-15));
#4887=DIRECTION('ref_axis',(3.49148133884313E-15,0.,-1.));
#4888=DIRECTION('',(0.,1.,0.));
#4889=DIRECTION('center_axis',(-1.,0.,-3.49148133884313E-15));
#4890=DIRECTION('ref_axis',(-3.49148133884313E-15,0.,1.));
#4891=DIRECTION('',(0.,1.,0.));
#4892=DIRECTION('center_axis',(0.,1.,0.));
#4893=DIRECTION('ref_axis',(0.,0.,1.));
#4894=DIRECTION('center_axis',(0.,-1.,0.));
#4895=DIRECTION('ref_axis',(0.,0.,-1.));
#4896=DIRECTION('center_axis',(0.,1.,0.));
#4897=DIRECTION('ref_axis',(0.,0.,1.));
#4898=DIRECTION('center_axis',(0.,1.,0.));
#4899=DIRECTION('ref_axis',(0.,0.,1.));
#4900=DIRECTION('center_axis',(0.,1.,0.));
#4901=DIRECTION('ref_axis',(3.43024899888577E-15,0.,-1.));
#4902=DIRECTION('center_axis',(0.,1.,0.));
#4903=DIRECTION('ref_axis',(0.,0.,1.));
#4904=DIRECTION('axis',(0.,0.,1.));
#4905=DIRECTION('refdir',(1.,0.,0.));
#4906=DIRECTION('center_axis',(1.,0.,0.));
#4907=DIRECTION('ref_axis',(0.,0.,-1.));
#4908=DIRECTION('center_axis',(1.,0.,0.));
#4909=DIRECTION('ref_axis',(0.,0.,-1.));
#4910=DIRECTION('',(0.,1.,1.85037170770859E-16));
#4911=DIRECTION('',(0.,0.,1.));
#4912=DIRECTION('center_axis',(1.,0.,0.));
#4913=DIRECTION('ref_axis',(0.,0.,-1.));
#4914=DIRECTION('center_axis',(1.,0.,0.));
#4915=DIRECTION('ref_axis',(0.,0.,-1.));
#4916=DIRECTION('',(0.,0.,1.));
#4917=DIRECTION('',(0.,-1.,-1.85037170770859E-16));
#4918=DIRECTION('center_axis',(1.,0.,0.));
#4919=DIRECTION('ref_axis',(0.,0.,-1.));
#4920=DIRECTION('center_axis',(1.,0.,0.));
#4921=DIRECTION('ref_axis',(0.,0.,-1.));
#4922=DIRECTION('',(0.,-1.,-1.8503717077086E-16));
#4923=DIRECTION('',(0.,0.,-1.));
#4924=DIRECTION('center_axis',(-1.,0.,0.));
#4925=DIRECTION('ref_axis',(0.,0.,1.));
#4926=DIRECTION('center_axis',(-1.,0.,0.));
#4927=DIRECTION('ref_axis',(0.,0.,1.));
#4928=DIRECTION('center_axis',(1.,0.,0.));
#4929=DIRECTION('ref_axis',(0.,0.,-1.));
#4930=DIRECTION('center_axis',(-1.,0.,0.));
#4931=DIRECTION('ref_axis',(0.,0.,1.));
#4932=DIRECTION('',(0.,1.,9.25185853854297E-17));
#4933=DIRECTION('',(0.,9.25185853854297E-17,-1.));
#4934=DIRECTION('',(0.,-1.,-1.85037170770859E-16));
#4935=DIRECTION('',(0.,0.,1.));
#4936=DIRECTION('center_axis',(-1.,0.,0.));
#4937=DIRECTION('ref_axis',(0.,0.,1.));
#4938=DIRECTION('center_axis',(-1.,0.,0.));
#4939=DIRECTION('ref_axis',(0.,0.,1.));
#4940=DIRECTION('',(1.,0.,0.));
#4941=DIRECTION('center_axis',(-1.,0.,0.));
#4942=DIRECTION('ref_axis',(0.,0.,1.));
#4943=DIRECTION('center_axis',(-1.,0.,0.));
#4944=DIRECTION('ref_axis',(0.,0.,1.));
#4945=DIRECTION('center_axis',(-1.,0.,0.));
#4946=DIRECTION('ref_axis',(0.,0.,1.));
#4947=DIRECTION('center_axis',(-1.,0.,0.));
#4948=DIRECTION('ref_axis',(0.,0.,1.));
#4949=DIRECTION('',(1.,0.,0.));
#4950=DIRECTION('center_axis',(0.,1.,0.));
#4951=DIRECTION('ref_axis',(0.,0.,1.));
#4952=DIRECTION('',(0.,1.,0.));
#4953=DIRECTION('center_axis',(-1.,0.,0.));
#4954=DIRECTION('ref_axis',(0.,0.,1.));
#4955=DIRECTION('center_axis',(0.,-1.,1.22464679914735E-16));
#4956=DIRECTION('ref_axis',(0.,-1.22464679914735E-16,-1.));
#4957=DIRECTION('center_axis',(0.,-1.44560289664734E-16,1.));
#4958=DIRECTION('ref_axis',(1.,0.,0.));
#4959=DIRECTION('',(-1.,0.,0.));
#4960=DIRECTION('',(0.,1.,0.));
#4961=DIRECTION('',(-1.,0.,0.));
#4962=DIRECTION('center_axis',(0.,-1.,0.));
#4963=DIRECTION('ref_axis',(0.,0.,-1.));
#4964=DIRECTION('',(-1.,0.,0.));
#4965=DIRECTION('center_axis',(0.,1.44560289664734E-16,-1.));
#4966=DIRECTION('ref_axis',(-1.,0.,0.));
#4967=DIRECTION('',(-1.,0.,0.));
#4968=DIRECTION('center_axis',(0.,1.,1.44560289664734E-16));
#4969=DIRECTION('ref_axis',(0.,-1.44560289664734E-16,1.));
#4970=DIRECTION('',(0.,1.85037170770859E-16,-1.));
#4971=DIRECTION('center_axis',(1.,0.,0.));
#4972=DIRECTION('ref_axis',(0.,0.,-1.));
#4973=DIRECTION('center_axis',(1.,0.,0.));
#4974=DIRECTION('ref_axis',(0.,0.,-1.));
#4975=DIRECTION('center_axis',(-1.,0.,0.));
#4976=DIRECTION('ref_axis',(0.,0.,1.));
#4977=DIRECTION('',(1.,0.,0.));
#4978=DIRECTION('center_axis',(1.,0.,0.));
#4979=DIRECTION('ref_axis',(0.,0.,-1.));
#4980=DIRECTION('center_axis',(1.,0.,0.));
#4981=DIRECTION('ref_axis',(0.,0.,-1.));
#4982=DIRECTION('axis',(0.,0.,1.));
#4983=DIRECTION('refdir',(1.,0.,0.));
#4984=DIRECTION('center_axis',(0.,1.,0.));
#4985=DIRECTION('ref_axis',(0.,0.,1.));
#4986=DIRECTION('center_axis',(0.,1.,0.));
#4987=DIRECTION('ref_axis',(0.,0.,1.));
#4988=DIRECTION('center_axis',(0.,1.,0.));
#4989=DIRECTION('ref_axis',(0.,0.,1.));
#4990=DIRECTION('center_axis',(0.,1.,0.));
#4991=DIRECTION('ref_axis',(0.,0.,1.));
#4992=DIRECTION('center_axis',(0.,1.,0.));
#4993=DIRECTION('ref_axis',(0.,0.,1.));
#4994=DIRECTION('center_axis',(0.,1.,0.));
#4995=DIRECTION('ref_axis',(0.,0.,1.));
#4996=DIRECTION('center_axis',(0.,-1.,0.));
#4997=DIRECTION('ref_axis',(0.,0.,-1.));
#4998=DIRECTION('',(0.,1.,0.));
#4999=DIRECTION('',(0.,1.,0.));
#5000=DIRECTION('center_axis',(0.,-1.,0.));
#5001=DIRECTION('ref_axis',(0.,0.,-1.));
#5002=DIRECTION('',(0.,-1.,0.));
#5003=DIRECTION('',(0.,-1.,0.));
#5004=DIRECTION('center_axis',(0.,0.,1.));
#5005=DIRECTION('ref_axis',(1.,0.,0.));
#5006=DIRECTION('',(-0.017854296416883,-2.18652069579638E-18,0.999840599345445));
#5007=DIRECTION('center_axis',(0.,0.,1.));
#5008=DIRECTION('ref_axis',(1.,0.,0.));
#5009=DIRECTION('',(-0.017854296416883,-2.18652069579638E-18,0.999840599345445));
#5010=DIRECTION('axis',(0.,0.,1.));
#5011=DIRECTION('refdir',(1.,0.,0.));
#5012=DIRECTION('center_axis',(1.,0.,0.));
#5013=DIRECTION('ref_axis',(0.,0.,-1.));
#5014=DIRECTION('center_axis',(-1.,0.,0.));
#5015=DIRECTION('ref_axis',(0.,0.,1.));
#5016=DIRECTION('',(-0.999840599345445,2.18652069579637E-18,-0.0178542964168829));
#5017=DIRECTION('center_axis',(-1.,0.,0.));
#5018=DIRECTION('ref_axis',(0.,0.,1.));
#5019=DIRECTION('center_axis',(1.,0.,0.));
#5020=DIRECTION('ref_axis',(0.,0.,-1.));
#5021=DIRECTION('center_axis',(-1.,0.,0.));
#5022=DIRECTION('ref_axis',(0.,0.,1.));
#5023=DIRECTION('axis',(0.,0.,1.));
#5024=DIRECTION('refdir',(1.,0.,0.));
#5025=DIRECTION('center_axis',(-3.43024899888577E-15,1.,0.));
#5026=DIRECTION('ref_axis',(0.,0.,1.));
#5027=DIRECTION('center_axis',(3.43024899888577E-15,-1.,0.));
#5028=DIRECTION('ref_axis',(1.,3.43024899888577E-15,0.));
#5029=DIRECTION('center_axis',(3.43024899888577E-15,-1.,0.));
#5030=DIRECTION('ref_axis',(1.,3.43024899888577E-15,0.));
#5031=DIRECTION('center_axis',(3.43024899888577E-15,-1.,0.));
#5032=DIRECTION('ref_axis',(1.,3.43024899888577E-15,0.));
#5033=DIRECTION('',(3.43024899888577E-15,-1.,0.));
#5034=DIRECTION('center_axis',(3.43024899888577E-15,-1.,0.));
#5035=DIRECTION('ref_axis',(1.,3.43024899888577E-15,0.));
#5036=DIRECTION('center_axis',(3.43024899888577E-15,-1.,0.));
#5037=DIRECTION('ref_axis',(1.,3.43024899888577E-15,0.));
#5038=DIRECTION('center_axis',(-3.43024899888577E-15,1.,0.));
#5039=DIRECTION('ref_axis',(-1.,-3.43024899888577E-15,0.));
#5040=DIRECTION('center_axis',(3.43024899888577E-15,-1.,0.));
#5041=DIRECTION('ref_axis',(1.,3.43024899888577E-15,0.));
#5042=DIRECTION('center_axis',(3.43024899888577E-15,-1.,0.));
#5043=DIRECTION('ref_axis',(1.,3.43024899888577E-15,0.));
#5044=DIRECTION('',(0.89442719099992,0.44721359549995,-1.09535739652841E-16));
#5045=DIRECTION('center_axis',(3.43024899888577E-15,-1.,0.));
#5046=DIRECTION('ref_axis',(1.,3.43024899888577E-15,0.));
#5047=DIRECTION('',(3.43024899888577E-15,-1.,0.));
#5048=DIRECTION('center_axis',(3.43024899888577E-15,-1.,0.));
#5049=DIRECTION('ref_axis',(1.,3.43024899888577E-15,0.));
#5050=DIRECTION('center_axis',(3.43024899888577E-15,-1.,0.));
#5051=DIRECTION('ref_axis',(0.,0.,-1.));
#5052=DIRECTION('center_axis',(3.43024899888577E-15,-1.,0.));
#5053=DIRECTION('ref_axis',(1.,3.43024899888577E-15,0.));
#5054=DIRECTION('center_axis',(-3.43024899888577E-15,1.,0.));
#5055=DIRECTION('ref_axis',(-1.,-3.43024899888577E-15,0.));
#5056=DIRECTION('center_axis',(3.43024899888577E-15,-1.,0.));
#5057=DIRECTION('ref_axis',(1.,3.43024899888577E-15,0.));
#5058=DIRECTION('',(-0.294085848837523,-0.95577900872195,3.60151293453408E-17));
#5059=DIRECTION('center_axis',(3.43024899888577E-15,-1.,0.));
#5060=DIRECTION('ref_axis',(0.,0.,-1.));
#5061=DIRECTION('center_axis',(3.43024899888577E-15,-1.,0.));
#5062=DIRECTION('ref_axis',(1.,3.43024899888577E-15,0.));
#5063=DIRECTION('center_axis',(3.43024899888577E-15,-1.,0.));
#5064=DIRECTION('ref_axis',(1.,3.43024899888577E-15,0.));
#5065=DIRECTION('',(-3.43024899888577E-15,1.,0.));
#5066=DIRECTION('center_axis',(3.43024899888577E-15,-1.,0.));
#5067=DIRECTION('ref_axis',(1.,3.43024899888577E-15,0.));
#5068=DIRECTION('center_axis',(3.43024899888577E-15,-1.,0.));
#5069=DIRECTION('ref_axis',(0.,0.,-1.));
#5070=DIRECTION('center_axis',(3.43024899888577E-15,-1.,0.));
#5071=DIRECTION('ref_axis',(1.,3.43024899888577E-15,0.));
#5072=DIRECTION('center_axis',(3.43024899888577E-15,-1.,0.));
#5073=DIRECTION('ref_axis',(1.,3.43024899888577E-15,0.));
#5074=DIRECTION('center_axis',(3.43024899888577E-15,-1.,0.));
#5075=DIRECTION('ref_axis',(1.,3.43024899888577E-15,0.));
#5076=DIRECTION('center_axis',(3.43024899888577E-15,-1.,0.));
#5077=DIRECTION('ref_axis',(1.,3.43024899888577E-15,0.));
#5078=DIRECTION('center_axis',(3.43024899888577E-15,-1.,0.));
#5079=DIRECTION('ref_axis',(1.,3.43024899888577E-15,0.));
#5080=DIRECTION('center_axis',(3.43024899888577E-15,-1.,0.));
#5081=DIRECTION('ref_axis',(1.,3.43024899888577E-15,0.));
#5082=DIRECTION('',(-3.43024899888577E-15,1.,0.));
#5083=DIRECTION('center_axis',(3.43024899888577E-15,-1.,0.));
#5084=DIRECTION('ref_axis',(1.,3.43024899888577E-15,0.));
#5085=DIRECTION('center_axis',(-3.43024899888577E-15,1.,0.));
#5086=DIRECTION('ref_axis',(0.,0.,1.));
#5087=DIRECTION('center_axis',(-3.43024899888577E-15,1.,5.91645678915759E-30));
#5088=DIRECTION('ref_axis',(3.49148133884313E-15,1.81438008200833E-29,-1.));
#5089=DIRECTION('center_axis',(-3.43024899888578E-15,1.,0.));
#5090=DIRECTION('ref_axis',(1.,3.43024899888578E-15,0.));
#5091=DIRECTION('center_axis',(-3.43024899888577E-15,1.,-5.91645678915759E-30));
#5092=DIRECTION('ref_axis',(-1.04744440165294E-14,-2.99767143983984E-29,
1.));
#5093=DIRECTION('center_axis',(-3.43024899888577E-15,1.,0.));
#5094=DIRECTION('ref_axis',(-1.,-3.43024899888577E-15,0.));
#5095=DIRECTION('center_axis',(3.43024899888577E-15,-1.,0.));
#5096=DIRECTION('ref_axis',(1.,3.43024899888577E-15,0.));
#5097=DIRECTION('center_axis',(3.43024899888577E-15,-1.,0.));
#5098=DIRECTION('ref_axis',(1.,3.43024899888577E-15,0.));
#5099=DIRECTION('',(-3.43024899888577E-15,1.,0.));
#5100=DIRECTION('center_axis',(-3.43024899888577E-15,1.,0.));
#5101=DIRECTION('ref_axis',(-1.,-3.43024899888577E-15,0.));
#5102=DIRECTION('',(-3.43024899888577E-15,1.,0.));
#5103=DIRECTION('center_axis',(-3.43024899888577E-15,1.,-5.91645678915759E-30));
#5104=DIRECTION('ref_axis',(-1.,-3.43024899888577E-15,0.));
#5105=DIRECTION('',(-3.43024899888577E-15,1.,-5.91645678915759E-30));
#5106=DIRECTION('center_axis',(-3.43024899888578E-15,1.,0.));
#5107=DIRECTION('ref_axis',(-1.,-3.43024899888578E-15,0.));
#5108=DIRECTION('',(-3.43024899888578E-15,1.,0.));
#5109=DIRECTION('center_axis',(-3.43024899888577E-15,1.,5.91645678915759E-30));
#5110=DIRECTION('ref_axis',(-1.,-3.43024899888577E-15,0.));
#5111=DIRECTION('',(-3.43024899888577E-15,1.,5.91645678915759E-30));
#5112=DIRECTION('axis',(0.,0.,1.));
#5113=DIRECTION('refdir',(1.,0.,0.));
#5114=DIRECTION('center_axis',(3.43024899888577E-15,-1.,0.));
#5115=DIRECTION('ref_axis',(1.,3.43024899888577E-15,0.));
#5116=DIRECTION('center_axis',(3.43024899888577E-15,-1.,0.));
#5117=DIRECTION('ref_axis',(1.,3.43024899888577E-15,0.));
#5118=DIRECTION('',(3.43024899888577E-15,-1.,0.));
#5119=DIRECTION('center_axis',(3.43024899888577E-15,-1.,0.));
#5120=DIRECTION('ref_axis',(1.,3.43024899888577E-15,0.));
#5121=DIRECTION('center_axis',(-3.43024899888577E-15,1.,0.));
#5122=DIRECTION('ref_axis',(0.,0.,1.));
#5123=DIRECTION('center_axis',(3.43024899888577E-15,-1.,0.));
#5124=DIRECTION('ref_axis',(1.,3.43024899888577E-15,0.));
#5125=DIRECTION('center_axis',(3.43024899888577E-15,-1.,0.));
#5126=DIRECTION('ref_axis',(1.,3.43024899888577E-15,0.));
#5127=DIRECTION('center_axis',(3.43024899888577E-15,-1.,0.));
#5128=DIRECTION('ref_axis',(1.,3.43024899888577E-15,0.));
#5129=DIRECTION('',(-3.43024899888577E-15,1.,0.));
#5130=DIRECTION('center_axis',(3.43024899888577E-15,-1.,0.));
#5131=DIRECTION('ref_axis',(0.,0.,-1.));
#5132=DIRECTION('center_axis',(3.43024899888577E-15,-1.,0.));
#5133=DIRECTION('ref_axis',(1.,3.43024899888577E-15,0.));
#5134=DIRECTION('center_axis',(3.43024899888577E-15,-1.,0.));
#5135=DIRECTION('ref_axis',(1.,3.43024899888577E-15,0.));
#5136=DIRECTION('center_axis',(3.43024899888577E-15,-1.,0.));
#5137=DIRECTION('ref_axis',(1.,3.43024899888577E-15,0.));
#5138=DIRECTION('',(-3.43024899888577E-15,1.,0.));
#5139=DIRECTION('center_axis',(3.43024899888577E-15,-1.,0.));
#5140=DIRECTION('ref_axis',(1.,3.43024899888577E-15,0.));
#5141=DIRECTION('',(-0.894427190999914,-0.447213595499962,-1.0953573965284E-16));
#5142=DIRECTION('axis',(0.,0.,1.));
#5143=DIRECTION('refdir',(1.,0.,0.));
#5144=DIRECTION('center_axis',(-0.866025403784441,0.,-0.499999999999995));
#5145=DIRECTION('ref_axis',(-0.499999999999995,0.,0.866025403784442));
#5146=DIRECTION('',(0.,-1.,0.));
#5147=DIRECTION('',(0.,-1.,0.));
#5148=DIRECTION('',(0.499999999999995,0.,-0.866025403784441));
#5149=DIRECTION('center_axis',(-0.866025403784438,0.,0.500000000000001));
#5150=DIRECTION('ref_axis',(0.500000000000001,0.,0.866025403784438));
#5151=DIRECTION('',(0.,-1.,0.));
#5152=DIRECTION('',(-0.500000000000001,0.,-0.866025403784438));
#5153=DIRECTION('center_axis',(3.29597460435593E-15,0.,1.));
#5154=DIRECTION('ref_axis',(1.,0.,-3.29597460435593E-15));
#5155=DIRECTION('',(-1.,0.,3.33066907387546E-15));
#5156=DIRECTION('',(0.,-1.,0.));
#5157=DIRECTION('center_axis',(0.866025403784442,0.,0.499999999999995));
#5158=DIRECTION('ref_axis',(0.499999999999995,0.,-0.866025403784442));
#5159=DIRECTION('',(0.,-1.,0.));
#5160=DIRECTION('',(-0.499999999999995,0.,0.866025403784441));
#5161=DIRECTION('center_axis',(0.866025403784435,0.,-0.500000000000007));
#5162=DIRECTION('ref_axis',(-0.500000000000007,0.,-0.866025403784435));
#5163=DIRECTION('',(0.,-1.,0.));
#5164=DIRECTION('',(0.500000000000007,0.,0.866025403784434));
#5165=DIRECTION('center_axis',(-1.04083408558608E-14,0.,-1.));
#5166=DIRECTION('ref_axis',(-1.,0.,1.04083408558608E-14));
#5167=DIRECTION('',(1.,0.,-1.04360964314765E-14));
#5168=DIRECTION('center_axis',(0.,1.,0.));
#5169=DIRECTION('ref_axis',(0.,0.,1.));
#5170=DIRECTION('center_axis',(0.,-1.,0.));
#5171=DIRECTION('ref_axis',(0.,0.,-1.));
#5172=DIRECTION('center_axis',(0.,-1.,0.));
#5173=DIRECTION('ref_axis',(0.,0.,-1.));
#5174=DIRECTION('center_axis',(0.,-1.,0.));
#5175=DIRECTION('ref_axis',(0.,0.,-1.));
#5176=DIRECTION('',(0.,-1.,0.));
#5177=DIRECTION('center_axis',(0.,-1.,0.));
#5178=DIRECTION('ref_axis',(0.,0.,-1.));
#5179=DIRECTION('center_axis',(0.,-1.,0.));
#5180=DIRECTION('ref_axis',(0.,0.,-1.));
#5181=DIRECTION('center_axis',(0.,-1.,0.));
#5182=DIRECTION('ref_axis',(0.,0.,-1.));
#5183=DIRECTION('center_axis',(0.,-1.,0.));
#5184=DIRECTION('ref_axis',(0.,0.,-1.));
#5185=DIRECTION('center_axis',(0.,-1.,0.));
#5186=DIRECTION('ref_axis',(0.,0.,-1.));
#5187=DIRECTION('center_axis',(0.,-1.,0.));
#5188=DIRECTION('ref_axis',(0.,0.,-1.));
#5189=DIRECTION('center_axis',(0.,-1.,0.));
#5190=DIRECTION('ref_axis',(0.,0.,-1.));
#5191=DIRECTION('center_axis',(0.,-1.,0.));
#5192=DIRECTION('ref_axis',(0.,0.,-1.));
#5193=DIRECTION('center_axis',(0.,-1.,0.));
#5194=DIRECTION('ref_axis',(0.,0.,-1.));
#5195=DIRECTION('center_axis',(0.,-1.,0.));
#5196=DIRECTION('ref_axis',(0.,0.,-1.));
#5197=DIRECTION('center_axis',(0.,-1.,0.));
#5198=DIRECTION('ref_axis',(0.,0.,-1.));
#5199=DIRECTION('center_axis',(0.,-1.,0.));
#5200=DIRECTION('ref_axis',(0.,0.,-1.));
#5201=DIRECTION('center_axis',(0.,-1.,0.));
#5202=DIRECTION('ref_axis',(0.,0.,-1.));
#5203=DIRECTION('center_axis',(0.,-1.,0.));
#5204=DIRECTION('ref_axis',(0.,0.,-1.));
#5205=DIRECTION('center_axis',(0.,1.,0.));
#5206=DIRECTION('ref_axis',(0.,0.,1.));
#5207=DIRECTION('center_axis',(0.,-1.,0.));
#5208=DIRECTION('ref_axis',(0.,0.,-1.));
#5209=DIRECTION('center_axis',(0.,1.,0.));
#5210=DIRECTION('ref_axis',(0.,0.,1.));
#5211=DIRECTION('center_axis',(0.,-1.,0.));
#5212=DIRECTION('ref_axis',(0.,0.,-1.));
#5213=DIRECTION('',(3.09767874512465E-17,0.967480747292902,-0.252944665129683));
#5214=DIRECTION('center_axis',(0.,-1.,0.));
#5215=DIRECTION('ref_axis',(0.,0.,-1.));
#5216=DIRECTION('center_axis',(0.,-1.,0.));
#5217=DIRECTION('ref_axis',(0.,0.,-1.));
#5218=DIRECTION('',(0.,-1.,0.));
#5219=DIRECTION('center_axis',(0.,-1.,0.));
#5220=DIRECTION('ref_axis',(0.,0.,-1.));
#5221=DIRECTION('center_axis',(0.,-1.,0.));
#5222=DIRECTION('ref_axis',(0.,0.,-1.));
#5223=DIRECTION('center_axis',(0.,1.,0.));
#5224=DIRECTION('ref_axis',(0.,0.,1.));
#5225=DIRECTION('',(0.,1.,0.));
#5226=DIRECTION('axis',(0.,0.,1.));
#5227=DIRECTION('refdir',(1.,0.,0.));
#5228=DIRECTION('center_axis',(0.,0.,1.));
#5229=DIRECTION('ref_axis',(1.,0.,0.));
#5230=DIRECTION('',(4.33942623640377E-17,-1.,0.));
#5231=DIRECTION('',(0.,1.,0.));
#5232=DIRECTION('',(-1.,0.,0.));
#5233=DIRECTION('center_axis',(0.,0.,1.));
#5234=DIRECTION('ref_axis',(1.,0.,0.));
#5235=DIRECTION('',(0.,1.,0.));
#5236=DIRECTION('',(4.33942623640377E-17,-1.,0.));
#5237=DIRECTION('',(-1.,0.,0.));
#5238=DIRECTION('center_axis',(-1.,0.,0.));
#5239=DIRECTION('ref_axis',(0.,0.,1.));
#5240=DIRECTION('center_axis',(-1.,0.,0.));
#5241=DIRECTION('ref_axis',(0.,0.,1.));
#5242=DIRECTION('center_axis',(1.,0.,0.));
#5243=DIRECTION('ref_axis',(0.,0.,-1.));
#5244=DIRECTION('center_axis',(-1.,0.,0.));
#5245=DIRECTION('ref_axis',(0.,0.,1.));
#5246=DIRECTION('',(0.,-3.49323812030503E-15,-1.));
#5247=DIRECTION('center_axis',(-1.,0.,0.));
#5248=DIRECTION('ref_axis',(0.,0.,1.));
#5249=DIRECTION('',(0.,-3.49323812030503E-15,-1.));
#5250=DIRECTION('center_axis',(1.,0.,0.));
#5251=DIRECTION('ref_axis',(0.,0.,-1.));
#5252=DIRECTION('center_axis',(1.,0.,0.));
#5253=DIRECTION('ref_axis',(0.,0.,-1.));
#5254=DIRECTION('center_axis',(-1.,0.,0.));
#5255=DIRECTION('ref_axis',(0.,0.,1.));
#5256=DIRECTION('',(0.,1.,0.));
#5257=DIRECTION('center_axis',(-1.,0.,0.));
#5258=DIRECTION('ref_axis',(0.,0.,1.));
#5259=DIRECTION('',(0.,1.,0.));
#5260=DIRECTION('center_axis',(1.,0.,0.));
#5261=DIRECTION('ref_axis',(0.,0.,-1.));
#5262=DIRECTION('center_axis',(1.,5.88949328263731E-17,0.));
#5263=DIRECTION('ref_axis',(0.,0.,-1.));
#5264=DIRECTION('',(6.50913935460565E-17,3.49323812030503E-15,1.));
#5265=DIRECTION('center_axis',(1.,5.88949328263731E-17,0.));
#5266=DIRECTION('ref_axis',(-5.88949328263731E-17,1.,0.));
#5267=DIRECTION('',(6.50913935460565E-17,3.49323812030503E-15,1.));
#5268=DIRECTION('center_axis',(-1.,2.05630558915701E-31,5.88949328263731E-17));
#5269=DIRECTION('ref_axis',(5.88949328263731E-17,0.,1.));
#5270=DIRECTION('center_axis',(-1.,2.05630558915701E-31,5.88949328263731E-17));
#5271=DIRECTION('ref_axis',(5.88949328263731E-17,0.,1.));
#5272=DIRECTION('center_axis',(1.,5.88949328263731E-17,0.));
#5273=DIRECTION('ref_axis',(0.,0.,-1.));
#5274=DIRECTION('center_axis',(1.,5.88949328263731E-17,0.));
#5275=DIRECTION('ref_axis',(-5.88949328263731E-17,1.,0.));
#5276=DIRECTION('center_axis',(-1.,-5.88949328263731E-17,0.));
#5277=DIRECTION('ref_axis',(5.88949328263731E-17,-1.,0.));
#5278=DIRECTION('center_axis',(1.,5.88949328263731E-17,0.));
#5279=DIRECTION('ref_axis',(0.,0.,-1.));
#5280=DIRECTION('',(4.33942623640377E-17,3.49323812030503E-15,1.));
#5281=DIRECTION('center_axis',(1.,5.88949328263731E-17,0.));
#5282=DIRECTION('ref_axis',(-5.88949328263731E-17,1.,0.));
#5283=DIRECTION('',(4.33942623640377E-17,3.49323812030503E-15,1.));
#5284=DIRECTION('center_axis',(-1.,2.05630558915701E-31,5.88949328263731E-17));
#5285=DIRECTION('ref_axis',(5.88949328263731E-17,0.,1.));
#5286=DIRECTION('center_axis',(0.,0.,1.));
#5287=DIRECTION('ref_axis',(1.,0.,0.));
#5288=DIRECTION('',(6.50913935460565E-17,-1.,0.));
#5289=DIRECTION('',(-1.,0.,0.));
#5290=DIRECTION('center_axis',(0.,0.,1.));
#5291=DIRECTION('ref_axis',(1.,0.,0.));
#5292=DIRECTION('',(6.50913935460565E-17,-1.,0.));
#5293=DIRECTION('',(-1.,0.,0.));
#5294=DIRECTION('center_axis',(0.,1.,-3.49148133884313E-15));
#5295=DIRECTION('ref_axis',(0.,3.49148133884313E-15,1.));
#5296=DIRECTION('',(-1.,0.,0.));
#5297=DIRECTION('center_axis',(0.,1.,-3.49148133884313E-15));
#5298=DIRECTION('ref_axis',(0.,3.49148133884313E-15,1.));
#5299=DIRECTION('',(-1.,0.,0.));
#5300=DIRECTION('center_axis',(0.,1.,-3.49148133884313E-15));
#5301=DIRECTION('ref_axis',(0.,3.49148133884313E-15,1.));
#5302=DIRECTION('',(0.,-3.49323812030503E-15,-1.));
#5303=DIRECTION('',(-1.,0.,0.));
#5304=DIRECTION('center_axis',(0.,1.,-3.49148133884313E-15));
#5305=DIRECTION('ref_axis',(0.,3.49148133884313E-15,1.));
#5306=DIRECTION('',(0.,-3.49323812030503E-15,-1.));
#5307=DIRECTION('',(-1.,0.,0.));
#5308=DIRECTION('center_axis',(-1.,0.,0.));
#5309=DIRECTION('ref_axis',(0.,0.,1.));
#5310=DIRECTION('center_axis',(0.,-1.,1.22464679914735E-16));
#5311=DIRECTION('ref_axis',(0.,-1.22464679914735E-16,-1.));
#5312=DIRECTION('center_axis',(1.,0.,0.));
#5313=DIRECTION('ref_axis',(0.,0.,1.));
#5314=DIRECTION('center_axis',(-1.,-5.88949328263731E-17,0.));
#5315=DIRECTION('ref_axis',(5.88949328263731E-17,-1.,0.));
#5316=DIRECTION('center_axis',(1.,0.,0.));
#5317=DIRECTION('ref_axis',(0.,0.,1.));
#5318=DIRECTION('center_axis',(1.,0.,0.));
#5319=DIRECTION('ref_axis',(0.,0.,1.));
#5320=DIRECTION('center_axis',(1.,0.,0.));
#5321=DIRECTION('ref_axis',(0.,0.,1.));
#5322=DIRECTION('center_axis',(1.,0.,0.));
#5323=DIRECTION('ref_axis',(0.,0.,-1.));
#5324=DIRECTION('center_axis',(-1.,0.,0.));
#5325=DIRECTION('ref_axis',(0.,0.,1.));
#5326=DIRECTION('center_axis',(-1.,0.,0.));
#5327=DIRECTION('ref_axis',(0.,0.,1.));
#5328=DIRECTION('center_axis',(1.,5.88949328263731E-17,0.));
#5329=DIRECTION('ref_axis',(0.,0.,-1.));
#5330=DIRECTION('center_axis',(1.,5.88949328263731E-17,0.));
#5331=DIRECTION('ref_axis',(-5.88949328263731E-17,1.,0.));
#5332=DIRECTION('center_axis',(-1.,0.,0.));
#5333=DIRECTION('ref_axis',(0.,0.,1.));
#5334=DIRECTION('center_axis',(1.,0.,0.));
#5335=DIRECTION('ref_axis',(0.,0.,-1.));
#5336=DIRECTION('',(1.,0.,0.));
#5337=DIRECTION('center_axis',(1.,5.88949328263731E-17,0.));
#5338=DIRECTION('ref_axis',(-5.88949328263731E-17,1.,0.));
#5339=DIRECTION('center_axis',(-1.,0.,0.));
#5340=DIRECTION('ref_axis',(0.,0.,1.));
#5341=DIRECTION('',(1.,0.,0.));
#5342=DIRECTION('center_axis',(1.,0.,0.));
#5343=DIRECTION('ref_axis',(0.,0.,-1.));
#5344=DIRECTION('center_axis',(-1.,0.,0.));
#5345=DIRECTION('ref_axis',(0.,0.,1.));
#5346=DIRECTION('center_axis',(1.,5.88949328263731E-17,0.));
#5347=DIRECTION('ref_axis',(-5.88949328263731E-17,1.,0.));
#5348=DIRECTION('center_axis',(-1.,0.,0.));
#5349=DIRECTION('ref_axis',(0.,0.,1.));
#5350=DIRECTION('center_axis',(1.,5.88949328263731E-17,0.));
#5351=DIRECTION('ref_axis',(-5.88949328263731E-17,1.,0.));
#5352=DIRECTION('center_axis',(-1.,0.,0.));
#5353=DIRECTION('ref_axis',(0.,0.,1.));
#5354=DIRECTION('center_axis',(1.,5.88949328263731E-17,0.));
#5355=DIRECTION('ref_axis',(-5.88949328263731E-17,1.,0.));
#5356=DIRECTION('center_axis',(1.,5.88949328263731E-17,0.));
#5357=DIRECTION('ref_axis',(-5.88949328263731E-17,1.,0.));
#5358=DIRECTION('center_axis',(-1.,0.,0.));
#5359=DIRECTION('ref_axis',(0.,0.,1.));
#5360=DIRECTION('center_axis',(1.,0.,0.));
#5361=DIRECTION('ref_axis',(0.,0.,-1.));
#5362=DIRECTION('',(0.,1.,-1.85037170770859E-16));
#5363=DIRECTION('',(0.,0.,-1.));
#5364=DIRECTION('',(0.,-1.,1.85037170770859E-16));
#5365=DIRECTION('',(0.,0.,1.));
#5366=DIRECTION('center_axis',(1.,0.,0.));
#5367=DIRECTION('ref_axis',(0.,0.,-1.));
#5368=DIRECTION('',(0.,0.,-1.));
#5369=DIRECTION('',(0.,1.,-1.85037170770859E-16));
#5370=DIRECTION('',(0.,0.,1.));
#5371=DIRECTION('',(0.,-1.,1.85037170770859E-16));
#5372=DIRECTION('center_axis',(0.,1.44560289664734E-16,1.));
#5373=DIRECTION('ref_axis',(1.,0.,0.));
#5374=DIRECTION('',(-1.,0.,0.));
#5375=DIRECTION('',(-1.,0.,0.));
#5376=DIRECTION('center_axis',(0.,-1.,0.));
#5377=DIRECTION('ref_axis',(0.,0.,-1.));
#5378=DIRECTION('',(-1.,0.,0.));
#5379=DIRECTION('center_axis',(0.,-1.44560289664734E-16,-1.));
#5380=DIRECTION('ref_axis',(-1.,0.,0.));
#5381=DIRECTION('',(-1.,0.,0.));
#5382=DIRECTION('center_axis',(0.,1.,0.));
#5383=DIRECTION('ref_axis',(0.,0.,1.));
#5384=DIRECTION('center_axis',(-1.,0.,0.));
#5385=DIRECTION('ref_axis',(0.,-3.67517835871524E-15,-1.));
#5386=DIRECTION('center_axis',(1.,5.88949328263731E-17,0.));
#5387=DIRECTION('ref_axis',(0.,0.,-1.));
#5388=DIRECTION('center_axis',(1.,5.88949328263731E-17,0.));
#5389=DIRECTION('ref_axis',(0.,0.,-1.));
#5390=DIRECTION('center_axis',(-1.,0.,0.));
#5391=DIRECTION('ref_axis',(0.,0.,1.));
#5392=DIRECTION('center_axis',(-1.,0.,0.));
#5393=DIRECTION('ref_axis',(0.,0.,1.));
#5394=DIRECTION('center_axis',(-1.,0.,0.));
#5395=DIRECTION('ref_axis',(0.,0.,1.));
#5396=DIRECTION('center_axis',(1.,5.88949328263731E-17,0.));
#5397=DIRECTION('ref_axis',(0.,0.,-1.));
#5398=DIRECTION('center_axis',(1.,5.88949328263731E-17,0.));
#5399=DIRECTION('ref_axis',(0.,3.43024899888577E-15,1.));
#5400=DIRECTION('axis',(0.,0.,1.));
#5401=DIRECTION('refdir',(1.,0.,0.));
#5402=DIRECTION('center_axis',(-0.866025403784439,0.,-0.5));
#5403=DIRECTION('ref_axis',(-0.5,0.,0.866025403784439));
#5404=DIRECTION('',(0.,-1.,0.));
#5405=DIRECTION('',(0.,-1.,0.));
#5406=DIRECTION('center_axis',(-0.866025403784439,0.,0.5));
#5407=DIRECTION('ref_axis',(0.5,0.,0.866025403784439));
#5408=DIRECTION('',(0.,-1.,0.));
#5409=DIRECTION('center_axis',(0.,0.,1.));
#5410=DIRECTION('ref_axis',(1.,0.,0.));
#5411=DIRECTION('',(0.,-1.,0.));
#5412=DIRECTION('center_axis',(0.866025403784439,0.,0.5));
#5413=DIRECTION('ref_axis',(0.5,0.,-0.866025403784439));
#5414=DIRECTION('',(0.,-1.,0.));
#5415=DIRECTION('center_axis',(0.866025403784439,0.,-0.5));
#5416=DIRECTION('ref_axis',(-0.5,0.,-0.866025403784439));
#5417=DIRECTION('',(0.,-1.,0.));
#5418=DIRECTION('center_axis',(1.44560289664734E-16,0.,-1.));
#5419=DIRECTION('ref_axis',(-1.,0.,-1.44560289664734E-16));
#5420=DIRECTION('center_axis',(0.,1.,0.));
#5421=DIRECTION('ref_axis',(0.,0.,1.));
#5422=DIRECTION('center_axis',(0.,1.,0.));
#5423=DIRECTION('ref_axis',(0.,0.,1.));
#5424=DIRECTION('center_axis',(0.,1.,0.));
#5425=DIRECTION('ref_axis',(0.,0.,1.));
#5426=DIRECTION('center_axis',(0.,1.,0.));
#5427=DIRECTION('ref_axis',(0.,0.,1.));
#5428=DIRECTION('center_axis',(0.,1.,0.));
#5429=DIRECTION('ref_axis',(0.,0.,1.));
#5430=DIRECTION('center_axis',(0.,-1.,0.));
#5431=DIRECTION('ref_axis',(0.,0.,-1.));
#5432=DIRECTION('center_axis',(0.,1.,0.));
#5433=DIRECTION('ref_axis',(0.,0.,1.));
#5434=DIRECTION('center_axis',(0.,1.,0.));
#5435=DIRECTION('ref_axis',(0.,0.,1.));
#5436=DIRECTION('center_axis',(0.,1.,0.));
#5437=DIRECTION('ref_axis',(0.,0.,1.));
#5438=DIRECTION('center_axis',(0.,1.,0.));
#5439=DIRECTION('ref_axis',(0.,0.,1.));
#5440=DIRECTION('center_axis',(0.,1.,0.));
#5441=DIRECTION('ref_axis',(0.,0.,1.));
#5442=DIRECTION('center_axis',(0.,1.,0.));
#5443=DIRECTION('ref_axis',(0.,0.,1.));
#5444=DIRECTION('center_axis',(0.,1.,0.));
#5445=DIRECTION('ref_axis',(0.,0.,1.));
#5446=DIRECTION('center_axis',(0.,1.,0.));
#5447=DIRECTION('ref_axis',(0.,0.,1.));
#5448=DIRECTION('center_axis',(0.,1.,0.));
#5449=DIRECTION('ref_axis',(0.,0.,1.));
#5450=DIRECTION('center_axis',(0.,1.,0.));
#5451=DIRECTION('ref_axis',(0.,0.,1.));
#5452=DIRECTION('center_axis',(0.,-1.,0.));
#5453=DIRECTION('ref_axis',(0.,0.,-1.));
#5454=DIRECTION('',(0.,-1.,0.));
#5455=DIRECTION('center_axis',(0.,-1.,0.));
#5456=DIRECTION('ref_axis',(0.,0.,1.));
#5457=DIRECTION('center_axis',(0.,-1.,0.));
#5458=DIRECTION('ref_axis',(0.,0.,1.));
#5459=DIRECTION('center_axis',(0.,-1.,0.));
#5460=DIRECTION('ref_axis',(0.,0.,1.));
#5461=DIRECTION('center_axis',(0.,-1.,0.));
#5462=DIRECTION('ref_axis',(0.,0.,1.));
#5463=DIRECTION('center_axis',(0.,-1.,0.));
#5464=DIRECTION('ref_axis',(0.,0.,1.));
#5465=DIRECTION('center_axis',(0.,-1.,0.));
#5466=DIRECTION('ref_axis',(0.,0.,1.));
#5467=DIRECTION('center_axis',(0.,1.,0.));
#5468=DIRECTION('ref_axis',(0.,0.,-1.));
#5469=DIRECTION('center_axis',(0.,1.,0.));
#5470=DIRECTION('ref_axis',(0.,0.,-1.));
#5471=DIRECTION('center_axis',(0.,1.,0.));
#5472=DIRECTION('ref_axis',(0.,0.,-1.));
#5473=DIRECTION('center_axis',(0.,1.,0.));
#5474=DIRECTION('ref_axis',(0.,0.,-1.));
#5475=DIRECTION('center_axis',(0.,1.,0.));
#5476=DIRECTION('ref_axis',(0.,0.,-1.));
#5477=DIRECTION('center_axis',(0.,1.,0.));
#5478=DIRECTION('ref_axis',(0.,0.,-1.));
#5479=DIRECTION('axis',(0.,0.,1.));
#5480=DIRECTION('refdir',(1.,0.,0.));
#5481=DIRECTION('center_axis',(-0.866025403784439,0.,-0.5));
#5482=DIRECTION('ref_axis',(-0.5,0.,0.866025403784439));
#5483=DIRECTION('',(0.,-1.,0.));
#5484=DIRECTION('',(0.5,0.,-0.866025403784439));
#5485=DIRECTION('',(0.,-1.,0.));
#5486=DIRECTION('center_axis',(-0.866025403784439,0.,0.5));
#5487=DIRECTION('ref_axis',(0.5,0.,0.866025403784439));
#5488=DIRECTION('',(-0.5,0.,-0.866025403784439));
#5489=DIRECTION('',(0.,-1.,0.));
#5490=DIRECTION('center_axis',(-1.44560289664734E-16,0.,1.));
#5491=DIRECTION('ref_axis',(1.,0.,1.44560289664734E-16));
#5492=DIRECTION('',(-1.,0.,-1.85037170770859E-16));
#5493=DIRECTION('',(0.,-1.,0.));
#5494=DIRECTION('center_axis',(0.866025403784439,0.,0.5));
#5495=DIRECTION('ref_axis',(0.5,0.,-0.866025403784439));
#5496=DIRECTION('',(-0.5,0.,0.866025403784439));
#5497=DIRECTION('',(0.,-1.,0.));
#5498=DIRECTION('center_axis',(0.866025403784439,0.,-0.5));
#5499=DIRECTION('ref_axis',(-0.5,0.,-0.866025403784439));
#5500=DIRECTION('',(0.5,0.,0.866025403784439));
#5501=DIRECTION('',(0.,-1.,0.));
#5502=DIRECTION('center_axis',(0.,0.,-1.));
#5503=DIRECTION('ref_axis',(-1.,0.,0.));
#5504=DIRECTION('',(1.,0.,0.));
#5505=DIRECTION('center_axis',(0.,-1.,0.));
#5506=DIRECTION('ref_axis',(0.,0.,-1.));
#5507=DIRECTION('center_axis',(0.,1.,0.));
#5508=DIRECTION('ref_axis',(0.,0.,1.));
#5509=DIRECTION('',(0.,1.,0.));
#5510=DIRECTION('center_axis',(0.,1.,0.));
#5511=DIRECTION('ref_axis',(0.,0.,1.));
#5512=DIRECTION('center_axis',(0.,1.,0.));
#5513=DIRECTION('ref_axis',(0.,0.,1.));
#5514=DIRECTION('center_axis',(0.,1.,0.));
#5515=DIRECTION('ref_axis',(0.,0.,1.));
#5516=DIRECTION('center_axis',(0.,-1.,0.));
#5517=DIRECTION('ref_axis',(0.,0.,1.));
#5518=DIRECTION('center_axis',(0.,1.,0.));
#5519=DIRECTION('ref_axis',(0.,0.,1.));
#5520=DIRECTION('center_axis',(0.,-1.,0.));
#5521=DIRECTION('ref_axis',(0.,0.,1.));
#5522=DIRECTION('center_axis',(0.,1.,0.));
#5523=DIRECTION('ref_axis',(0.,0.,1.));
#5524=DIRECTION('center_axis',(0.,-1.,0.));
#5525=DIRECTION('ref_axis',(0.,0.,1.));
#5526=DIRECTION('center_axis',(0.,1.,0.));
#5527=DIRECTION('ref_axis',(0.,0.,1.));
#5528=DIRECTION('center_axis',(0.,-1.,0.));
#5529=DIRECTION('ref_axis',(0.,0.,1.));
#5530=DIRECTION('center_axis',(0.,1.,0.));
#5531=DIRECTION('ref_axis',(0.,0.,1.));
#5532=DIRECTION('center_axis',(0.,-1.,0.));
#5533=DIRECTION('ref_axis',(0.,0.,1.));
#5534=DIRECTION('center_axis',(0.,1.,0.));
#5535=DIRECTION('ref_axis',(0.,0.,1.));
#5536=DIRECTION('center_axis',(0.,-1.,0.));
#5537=DIRECTION('ref_axis',(0.,0.,1.));
#5538=DIRECTION('center_axis',(0.,1.,0.));
#5539=DIRECTION('ref_axis',(0.,0.,1.));
#5540=DIRECTION('center_axis',(0.,1.,0.));
#5541=DIRECTION('ref_axis',(0.,0.,1.));
#5542=DIRECTION('',(0.,0.,1.));
#5543=DIRECTION('',(1.,0.,0.));
#5544=DIRECTION('',(0.,0.,1.));
#5545=DIRECTION('',(1.,0.,0.));
#5546=DIRECTION('',(1.,3.43024899888554E-15,3.08148791101958E-33));
#5547=DIRECTION('',(-3.43024899888574E-15,1.,1.17373598748271E-16));
#5548=DIRECTION('',(0.,0.,1.));
#5549=DIRECTION('',(1.,0.,0.));
#5550=DIRECTION('',(-0.966606997534245,-0.256263365149669,1.34143668053289E-17));
#5551=DIRECTION('',(1.38777878078145E-17,-5.45519656747685E-32,1.));
#5552=DIRECTION('',(0.,0.,1.));
#5553=DIRECTION('',(1.,0.,0.));
#5554=DIRECTION('',(0.,0.,1.));
#5555=DIRECTION('',(1.,0.,0.));
#5556=DIRECTION('',(2.77555756156289E-17,-1.57772181044202E-30,-1.));
#5557=DIRECTION('',(-1.,-3.43024899888576E-15,-2.77555756156289E-17));
#5558=DIRECTION('',(1.4456028968001E-16,1.17373598719963E-16,-1.));
#5559=DIRECTION('',(3.43024899888574E-15,-1.,-1.17373598719945E-16));
#5560=DIRECTION('',(0.,0.,1.));
#5561=DIRECTION('',(1.,0.,0.));
#5562=DIRECTION('',(-1.11022302462516E-16,5.52202633654708E-30,-1.));
#5563=DIRECTION('',(-1.,-3.43024899888577E-15,1.11022302462516E-16));
#5564=DIRECTION('',(1.,3.43024899888577E-15,3.38045903638062E-15));
#5565=DIRECTION('',(3.38045903638062E-15,5.93005309989206E-30,-1.));
#5566=DIRECTION('',(0.,0.,1.));
#5567=DIRECTION('',(1.,0.,0.));
#5568=DIRECTION('',(-1.,-3.43024899888576E-15,-1.03634217140669E-14));
#5569=DIRECTION('',(-1.03634217140669E-14,-4.14287938348376E-29,1.));
#5570=CARTESIAN_POINT('',(0.,0.,0.));
#5571=CARTESIAN_POINT('',(0.,0.,0.));
#5572=CARTESIAN_POINT('Origin',(-2.22044604925031E-13,65.9999999999997,
0.));
#5573=CARTESIAN_POINT('',(84.5218814663268,63.9999999999999,24.4959497344398));
#5574=CARTESIAN_POINT('',(84.5218814663268,63.9999999999999,-24.4959497344398));
#5575=CARTESIAN_POINT('Origin',(-2.19535935928688E-13,63.9999999999996,
0.));
#5576=CARTESIAN_POINT('',(89.1964124839111,65.9999999999999,12.));
#5577=CARTESIAN_POINT('Ctrl Pts',(84.5218814663268,64.,24.4959497344398));
#5578=CARTESIAN_POINT('Ctrl Pts',(84.9038127722375,64.,23.9157900880511));
#5579=CARTESIAN_POINT('Ctrl Pts',(85.2940373732189,64.0317096659725,23.2792569494813));
#5580=CARTESIAN_POINT('Ctrl Pts',(87.3160364923004,64.3594769795007,19.6445825482463));
#5581=CARTESIAN_POINT('Ctrl Pts',(88.643006529544,65.1313887892092,16.0828655187997));
#5582=CARTESIAN_POINT('Ctrl Pts',(89.1937556100172,65.9958068625112,12.0197115471009));
#5583=CARTESIAN_POINT('Ctrl Pts',(89.1950864974236,65.9979034312765,12.0098561031404));
#5584=CARTESIAN_POINT('Ctrl Pts',(89.196412483911,66.,12.));
#5585=CARTESIAN_POINT('',(-90.0000000000005,65.9999999999993,-1.10218211923262E-14));
#5586=CARTESIAN_POINT('Origin',(-2.2639643392646E-13,65.9999999999996,0.));
#5587=CARTESIAN_POINT('',(89.196412483911,65.9999999999999,-12.));
#5588=CARTESIAN_POINT('Origin',(-2.2639643392646E-13,65.9999999999996,0.));
#5589=CARTESIAN_POINT('Ctrl Pts',(84.5218814663268,64.,-24.4959497344398));
#5590=CARTESIAN_POINT('Ctrl Pts',(84.7701310773201,64.,-24.1188546801693));
#5591=CARTESIAN_POINT('Ctrl Pts',(85.0220290607656,64.0133758231304,-23.7177022308239));
#5592=CARTESIAN_POINT('Ctrl Pts',(86.1522258688305,64.1327263249616,-21.8101284980407));
#5593=CARTESIAN_POINT('Ctrl Pts',(86.9849682511504,64.379237185943,-20.1156541149184));
#5594=CARTESIAN_POINT('Ctrl Pts',(88.4016861752627,65.0999401070311,-16.1941739449509));
#5595=CARTESIAN_POINT('Ctrl Pts',(88.9080060701816,65.5473139367667,-14.1278301420605));
#5596=CARTESIAN_POINT('Ctrl Pts',(89.1937556100206,65.9958068625089,-12.0197115470756));
#5597=CARTESIAN_POINT('Ctrl Pts',(89.195086497424,65.9979034312771,-12.0098561031374));
#5598=CARTESIAN_POINT('Ctrl Pts',(89.196412483911,66.,-12.));
#5599=CARTESIAN_POINT('Origin',(-90.0010000000005,21.9999999999997,0.));
#5600=CARTESIAN_POINT('',(41.13395568512,21.9999999999999,38.));
#5601=CARTESIAN_POINT('',(41.1339720798708,21.9999999999999,-38.));
#5602=CARTESIAN_POINT('Ctrl Pts',(41.13395568512,21.9999999999997,38.));
#5603=CARTESIAN_POINT('Ctrl Pts',(41.13395568512,24.5049526391433,38.));
#5604=CARTESIAN_POINT('Ctrl Pts',(41.3698859733185,27.0457064732876,37.7490333835055));
#5605=CARTESIAN_POINT('Ctrl Pts',(42.2668103555191,32.0237155256726,36.7419897039594));
#5606=CARTESIAN_POINT('Ctrl Pts',(42.9248433632201,34.4616282231014,35.9865277696606));
#5607=CARTESIAN_POINT('Ctrl Pts',(44.4913270859975,39.0947019839386,34.0307796957095));
#5608=CARTESIAN_POINT('Ctrl Pts',(45.398690949306,41.2947913266836,32.8288186947832));
#5609=CARTESIAN_POINT('Ctrl Pts',(47.2681227122205,45.3564353734818,30.0748605376039));
#5610=CARTESIAN_POINT('Ctrl Pts',(48.2290184872111,47.2180132517743,28.5221020796692));
#5611=CARTESIAN_POINT('Ctrl Pts',(50.0250804079731,50.5021494267391,25.2379659817043));
#5612=CARTESIAN_POINT('Ctrl Pts',(50.9300602235279,52.0511318891308,23.387202355214));
#5613=CARTESIAN_POINT('Ctrl Pts',(52.6061045330048,54.8116067028424,19.3243428839503));
#5614=CARTESIAN_POINT('Ctrl Pts',(53.3762495117073,56.0232593397458,17.1119766759343));
#5615=CARTESIAN_POINT('Ctrl Pts',(54.6519856594464,57.9916316933046,12.4500772721613));
#5616=CARTESIAN_POINT('Ctrl Pts',(55.1581885566719,58.7499727721315,9.99553864743798));
#5617=CARTESIAN_POINT('Ctrl Pts',(55.8324050725756,59.7543646835585,5.00791763065262));
#5618=CARTESIAN_POINT('Ctrl Pts',(56.0000358879638,59.9999999999997,2.47469983355769));
#5619=CARTESIAN_POINT('Ctrl Pts',(56.0000366722163,59.9999999999997,-2.47469958668799));
#5620=CARTESIAN_POINT('Ctrl Pts',(55.8324066922941,59.7543647315935,-5.00791719772311));
#5621=CARTESIAN_POINT('Ctrl Pts',(55.1581918868508,58.7499729504375,-9.99553795640079));
#5622=CARTESIAN_POINT('Ctrl Pts',(54.6519898647332,57.9916319532894,-12.4500765088443));
#5623=CARTESIAN_POINT('Ctrl Pts',(53.3762554539761,56.0232597504026,-17.1119758509008));
#5624=CARTESIAN_POINT('Ctrl Pts',(52.6061113388684,54.8116071817857,-19.3243420707035));
#5625=CARTESIAN_POINT('Ctrl Pts',(50.9300687027128,52.0511324690522,-23.3872016100264));
#5626=CARTESIAN_POINT('Ctrl Pts',(50.0250896973938,50.5021500393159,-25.2379652925953));
#5627=CARTESIAN_POINT('Ctrl Pts',(48.2290292589987,47.2180138110437,-28.5221015978674));
#5628=CARTESIAN_POINT('Ctrl Pts',(47.2681342172102,45.3564358424301,-30.0748601848596));
#5629=CARTESIAN_POINT('Ctrl Pts',(45.3987038776794,41.2947915957089,-32.8288185471517));
#5630=CARTESIAN_POINT('Ctrl Pts',(44.4913407056712,39.0947021428606,-34.030779623489));
#5631=CARTESIAN_POINT('Ctrl Pts',(42.9248582173494,34.4616281959662,-35.9865277862501));
#5632=CARTESIAN_POINT('Ctrl Pts',(42.2668257527207,32.0237154223944,-36.7419897336045));
#5633=CARTESIAN_POINT('Ctrl Pts',(41.369902143272,27.0457063249303,-37.7490334047659));
#5634=CARTESIAN_POINT('Ctrl Pts',(41.1339720798708,24.504952523231,-38.));
#5635=CARTESIAN_POINT('Ctrl Pts',(41.1339720798708,21.9999999999997,-38.));
#5636=CARTESIAN_POINT('',(59.4642749892742,22.,-38.));
#5637=CARTESIAN_POINT('',(41.1339720798708,21.9999999999999,-38.));
#5638=CARTESIAN_POINT('',(89.1964124839111,58.0555127546396,-12.));
#5639=CARTESIAN_POINT('Ctrl Pts',(89.1964124839111,58.0555127546396,-12.));
#5640=CARTESIAN_POINT('Ctrl Pts',(89.1190199896171,57.8640542974771,-12.5752610703505));
#5641=CARTESIAN_POINT('Ctrl Pts',(89.0250779102713,57.6584422520644,-13.1470340093289));
#5642=CARTESIAN_POINT('Ctrl Pts',(88.5525797543681,56.7159929487085,-15.5825558333806));
#5643=CARTESIAN_POINT('Ctrl Pts',(88.0143914281752,55.8427290142663,-17.3935784710887));
#5644=CARTESIAN_POINT('Ctrl Pts',(86.6610431662391,53.8665957514274,-20.7939147542697));
#5645=CARTESIAN_POINT('Ctrl Pts',(85.8451876894935,52.76239978252,-22.3861978423013));
#5646=CARTESIAN_POINT('Ctrl Pts',(84.0425817165657,50.4264221335801,-25.2864710591156));
#5647=CARTESIAN_POINT('Ctrl Pts',(83.056053899723,49.1947849510484,-26.5947159612042));
#5648=CARTESIAN_POINT('Ctrl Pts',(80.5654234362146,46.1505453853588,-29.4436626273688));
#5649=CARTESIAN_POINT('Ctrl Pts',(78.8977661523696,44.1685496793139,-30.9617789456884));
#5650=CARTESIAN_POINT('Ctrl Pts',(75.3156320753682,39.9826685922426,-33.5663519067529));
#5651=CARTESIAN_POINT('Ctrl Pts',(73.4012521028471,37.7788157607244,-34.6529940162392));
#5652=CARTESIAN_POINT('Ctrl Pts',(69.4585378993709,33.2773576738104,-36.367872488476));
#5653=CARTESIAN_POINT('Ctrl Pts',(67.429009853746,30.978347996818,-36.9965695983663));
#5654=CARTESIAN_POINT('Ctrl Pts',(63.3934115878716,26.4218766001607,-37.8127478744626));
#5655=CARTESIAN_POINT('Ctrl Pts',(61.3873583010373,24.164358858964,-38.));
#5656=CARTESIAN_POINT('Ctrl Pts',(59.4642749892743,21.9999999999999,-38.));
#5657=CARTESIAN_POINT('',(89.1964124839111,58.0555127546396,12.));
#5658=CARTESIAN_POINT('Ctrl Pts',(89.1964124839111,58.0555127546396,-12.));
#5659=CARTESIAN_POINT('Ctrl Pts',(89.4006007095317,58.5606465276845,-10.4822619002651));
#5660=CARTESIAN_POINT('Ctrl Pts',(89.5691633283084,58.9690896845165,-8.93349037421489));
#5661=CARTESIAN_POINT('Ctrl Pts',(89.9001752372116,59.765576470203,-4.90814187236786));
#5662=CARTESIAN_POINT('Ctrl Pts',(90.0000000000001,59.9999999999997,-2.41748397242429));
#5663=CARTESIAN_POINT('Ctrl Pts',(90.0000000000001,59.9999999999997,2.41748397242427));
#5664=CARTESIAN_POINT('Ctrl Pts',(89.9001752372116,59.7655764702031,4.90814187236785));
#5665=CARTESIAN_POINT('Ctrl Pts',(89.5691633283084,58.9690896845165,8.93349037421488));
#5666=CARTESIAN_POINT('Ctrl Pts',(89.4006007095317,58.5606465276845,10.4822619002651));
#5667=CARTESIAN_POINT('Ctrl Pts',(89.1964124839111,58.0555127546396,12.));
#5668=CARTESIAN_POINT('',(59.4642749892742,22.,38.));
#5669=CARTESIAN_POINT('Ctrl Pts',(89.1964124839111,58.0555127546396,12.));
#5670=CARTESIAN_POINT('Ctrl Pts',(89.1190199896171,57.8640542974771,12.5752610703505));
#5671=CARTESIAN_POINT('Ctrl Pts',(89.0250779102713,57.6584422520644,13.1470340093289));
#5672=CARTESIAN_POINT('Ctrl Pts',(88.5525797543681,56.7159929487085,15.5825558333806));
#5673=CARTESIAN_POINT('Ctrl Pts',(88.0143914281752,55.8427290142662,17.3935784710887));
#5674=CARTESIAN_POINT('Ctrl Pts',(86.6610431662391,53.8665957514274,20.7939147542697));
#5675=CARTESIAN_POINT('Ctrl Pts',(85.8451876894935,52.76239978252,22.3861978423013));
#5676=CARTESIAN_POINT('Ctrl Pts',(84.0425817165657,50.4264221335801,25.2864710591156));
#5677=CARTESIAN_POINT('Ctrl Pts',(83.0560538997229,49.1947849510483,26.5947159612043));
#5678=CARTESIAN_POINT('Ctrl Pts',(80.5654234362146,46.1505453853588,29.4436626273688));
#5679=CARTESIAN_POINT('Ctrl Pts',(78.8977661523695,44.1685496793138,30.9617789456885));
#5680=CARTESIAN_POINT('Ctrl Pts',(75.3156320753681,39.9826685922425,33.5663519067529));
#5681=CARTESIAN_POINT('Ctrl Pts',(73.4012521028471,37.7788157607244,34.6529940162392));
#5682=CARTESIAN_POINT('Ctrl Pts',(69.4585378993709,33.2773576738104,36.367872488476));
#5683=CARTESIAN_POINT('Ctrl Pts',(67.429009853746,30.978347996818,36.9965695983663));
#5684=CARTESIAN_POINT('Ctrl Pts',(63.3934115878716,26.4218766001607,37.8127478744626));
#5685=CARTESIAN_POINT('Ctrl Pts',(61.3873583010373,24.164358858964,38.));
#5686=CARTESIAN_POINT('Ctrl Pts',(59.4642749892743,21.9999999999999,38.));
#5687=CARTESIAN_POINT('',(114.,21.9999999999997,38.));
#5688=CARTESIAN_POINT('',(-90.0010000000005,21.9999999999997,38.));
#5689=CARTESIAN_POINT('Origin',(114.,21.9999999999997,0.));
#5690=CARTESIAN_POINT('',(59.4642749892742,22.,38.));
#5691=CARTESIAN_POINT('',(52.1152568831818,-10.0000000000004,20.493901531919));
#5692=CARTESIAN_POINT('Ctrl Pts',(41.1339276024063,21.9999999999997,38.));
#5693=CARTESIAN_POINT('Ctrl Pts',(41.1339276024063,19.4950474188123,38.));
#5694=CARTESIAN_POINT('Ctrl Pts',(41.3698577782062,16.9542936008905,37.7490333941357));
#5695=CARTESIAN_POINT('Ctrl Pts',(42.2667817740307,11.9762845259659,36.741989718782));
#5696=CARTESIAN_POINT('Ctrl Pts',(42.9248145101955,9.53837179046566,35.9865277779553));
#5697=CARTESIAN_POINT('Ctrl Pts',(44.491297615745,4.90529793659982,34.0307796595992));
#5698=CARTESIAN_POINT('Ctrl Pts',(45.3986611334033,2.70520853880316,32.8288186209674));
#5699=CARTESIAN_POINT('Ctrl Pts',(47.2680921846259,-1.3564356079566,30.0748603612317));
#5700=CARTESIAN_POINT('Ctrl Pts',(48.2289875930154,-3.21801353140966,28.5221018387682));
#5701=CARTESIAN_POINT('Ctrl Pts',(50.0250487725939,-6.50214973302819,25.2379656371497));
#5702=CARTESIAN_POINT('Ctrl Pts',(50.9300281830307,-8.05113217909215,23.3872019826201));
#5703=CARTESIAN_POINT('Ctrl Pts',(51.8851439691307,-9.62422563773273,21.0719271623962));
#5704=CARTESIAN_POINT('Ctrl Pts',(52.0009460104357,-9.81383310944727,20.7845899832333));
#5705=CARTESIAN_POINT('Ctrl Pts',(52.1152568831818,-10.0000000000004,20.493901531919));
#5706=CARTESIAN_POINT('',(52.1152568831817,-10.0000000000002,-20.4939015319188));
#5707=CARTESIAN_POINT('Ctrl Pts',(52.1152568831816,-10.0000000000005,20.493901531919));
#5708=CARTESIAN_POINT('Ctrl Pts',(52.9920598772145,-11.427962914687,18.2642229517423));
#5709=CARTESIAN_POINT('Ctrl Pts',(53.4487275116836,-12.800109304042,15.628623783461));
#5710=CARTESIAN_POINT('Ctrl Pts',(53.6428401425395,-14.8055170663448,9.84683279520228));
#5711=CARTESIAN_POINT('Ctrl Pts',(53.4915500984615,-15.4263415985926,7.14093283352039));
#5712=CARTESIAN_POINT('Ctrl Pts',(53.3537086148268,-15.8453555314119,3.53009503335275));
#5713=CARTESIAN_POINT('Ctrl Pts',(53.3258483126282,-15.9159138020226,2.67163594799237));
#5714=CARTESIAN_POINT('Ctrl Pts',(53.2987508848524,-15.9829447710969,1.26141826952118));
#5715=CARTESIAN_POINT('Ctrl Pts',(53.2926607217507,-15.9972472233255,0.715583753770389));
#5716=CARTESIAN_POINT('Ctrl Pts',(53.2906987538236,-16.0019108788503,-0.356739054022367));
#5717=CARTESIAN_POINT('Ctrl Pts',(53.294321434229,-15.99345855971,-0.881048064909989));
#5718=CARTESIAN_POINT('Ctrl Pts',(53.3135705802987,-15.9465857713104,-2.14429489073831));
#5719=CARTESIAN_POINT('Ctrl Pts',(53.3333698832412,-15.8978903517419,-2.88150257955492));
#5720=CARTESIAN_POINT('Ctrl Pts',(53.3892695140974,-15.7411204686839,-4.51882129056692));
#5721=CARTESIAN_POINT('Ctrl Pts',(53.4277924573997,-15.6228736964551,-5.41747303556089));
#5722=CARTESIAN_POINT('Ctrl Pts',(53.5329994424471,-15.1901728977435,-7.98473738653545));
#5723=CARTESIAN_POINT('Ctrl Pts',(53.5944639440763,-14.7956338714779,-9.64539296566124));
#5724=CARTESIAN_POINT('Ctrl Pts',(53.5480496875213,-13.1924305377066,-14.7997725951247));
#5725=CARTESIAN_POINT('Ctrl Pts',(53.1488326938255,-11.7260326931231,-17.7622050761178));
#5726=CARTESIAN_POINT('Ctrl Pts',(52.1679065869839,-10.0863024534087,-20.358676489776));
#5727=CARTESIAN_POINT('Ctrl Pts',(52.141763209695,-10.0431682504778,-20.4264968938551));
#5728=CARTESIAN_POINT('Ctrl Pts',(52.1152568831816,-10.0000000000005,-20.493901531919));
#5729=CARTESIAN_POINT('Ctrl Pts',(52.1152568831818,-10.0000000000004,-20.493901531919));
#5730=CARTESIAN_POINT('Ctrl Pts',(52.0009460104357,-9.81383310944727,-20.7845899832333));
#5731=CARTESIAN_POINT('Ctrl Pts',(51.8851439691307,-9.62422563773273,-21.0719271623962));
#5732=CARTESIAN_POINT('Ctrl Pts',(50.9300281830307,-8.05113217909215,-23.3872019826201));
#5733=CARTESIAN_POINT('Ctrl Pts',(50.0250487725939,-6.50214973302819,-25.2379656371497));
#5734=CARTESIAN_POINT('Ctrl Pts',(48.2289875930154,-3.21801353140967,-28.5221018387682));
#5735=CARTESIAN_POINT('Ctrl Pts',(47.2680921846259,-1.3564356079566,-30.0748603612317));
#5736=CARTESIAN_POINT('Ctrl Pts',(45.3986611334033,2.70520853880316,-32.8288186209674));
#5737=CARTESIAN_POINT('Ctrl Pts',(44.491297615745,4.90529793659981,-34.0307796595992));
#5738=CARTESIAN_POINT('Ctrl Pts',(42.9248145101955,9.53837179046566,-35.9865277779553));
#5739=CARTESIAN_POINT('Ctrl Pts',(42.2667817740307,11.9762845259659,-36.741989718782));
#5740=CARTESIAN_POINT('Ctrl Pts',(41.3698577782062,16.9542936008905,-37.7490333941357));
#5741=CARTESIAN_POINT('Ctrl Pts',(41.1339276024063,19.4950474188123,-38.));
#5742=CARTESIAN_POINT('Ctrl Pts',(41.1339276024063,24.5049525811872,-38.));
#5743=CARTESIAN_POINT('Ctrl Pts',(41.3698577782062,27.045706399109,-37.7490333941357));
#5744=CARTESIAN_POINT('Ctrl Pts',(42.2667817740307,32.0237154740336,-36.741989718782));
#5745=CARTESIAN_POINT('Ctrl Pts',(42.9248145101955,34.4616282095338,-35.9865277779553));
#5746=CARTESIAN_POINT('Ctrl Pts',(44.4912976157449,39.0947020633997,-34.0307796595992));
#5747=CARTESIAN_POINT('Ctrl Pts',(45.3986611334032,41.2947914611964,-32.8288186209674));
#5748=CARTESIAN_POINT('Ctrl Pts',(47.2680921846258,45.3564356079561,-30.0748603612317));
#5749=CARTESIAN_POINT('Ctrl Pts',(48.2289875930153,47.2180135314092,-28.5221018387682));
#5750=CARTESIAN_POINT('Ctrl Pts',(50.0250487725937,50.5021497330277,-25.2379656371497));
#5751=CARTESIAN_POINT('Ctrl Pts',(50.9300281830306,52.0511321790916,-23.38720198262));
#5752=CARTESIAN_POINT('Ctrl Pts',(52.6060716558467,54.8116069423141,-19.3243424773267));
#5753=CARTESIAN_POINT('Ctrl Pts',(53.3762162027518,56.0232595450743,-17.1119762634174));
#5754=CARTESIAN_POINT('Ctrl Pts',(54.6519514819998,57.991631823297,-12.4500768905027));
#5755=CARTESIAN_POINT('Ctrl Pts',(55.1581539416713,58.7499728612845,-9.99553830191928));
#5756=CARTESIAN_POINT('Ctrl Pts',(55.8323696023447,59.754364707576,-5.0079174141878));
#5757=CARTESIAN_POINT('Ctrl Pts',(55.9999999999999,59.9999999999997,-2.47469971012283));
#5758=CARTESIAN_POINT('Ctrl Pts',(55.9999999999999,59.9999999999997,2.4746997101228));
#5759=CARTESIAN_POINT('Ctrl Pts',(55.8323696023447,59.754364707576,5.00791741418778));
#5760=CARTESIAN_POINT('Ctrl Pts',(55.1581539416713,58.7499728612845,9.99553830191926));
#5761=CARTESIAN_POINT('Ctrl Pts',(54.6519514819998,57.991631823297,12.4500768905027));
#5762=CARTESIAN_POINT('Ctrl Pts',(53.3762162027518,56.0232595450743,17.1119762634174));
#5763=CARTESIAN_POINT('Ctrl Pts',(52.6060716558467,54.8116069423141,19.3243424773267));
#5764=CARTESIAN_POINT('Ctrl Pts',(50.9300281830306,52.0511321790916,23.38720198262));
#5765=CARTESIAN_POINT('Ctrl Pts',(50.0250487725937,50.5021497330277,25.2379656371497));
#5766=CARTESIAN_POINT('Ctrl Pts',(48.2289875930153,47.2180135314091,28.5221018387682));
#5767=CARTESIAN_POINT('Ctrl Pts',(47.2680921846258,45.3564356079561,30.0748603612317));
#5768=CARTESIAN_POINT('Ctrl Pts',(45.3986611334032,41.2947914611964,32.8288186209674));
#5769=CARTESIAN_POINT('Ctrl Pts',(44.491297615745,39.0947020633997,34.0307796595992));
#5770=CARTESIAN_POINT('Ctrl Pts',(42.9248145101955,34.4616282095338,35.9865277779553));
#5771=CARTESIAN_POINT('Ctrl Pts',(42.2667817740307,32.0237154740336,36.741989718782));
#5772=CARTESIAN_POINT('Ctrl Pts',(41.3698577782062,27.045706399109,37.7490333941357));
#5773=CARTESIAN_POINT('Ctrl Pts',(41.1339276024063,24.5049525811872,38.));
#5774=CARTESIAN_POINT('Ctrl Pts',(41.1339276024063,21.9999999999997,38.));
#5775=CARTESIAN_POINT('Origin',(-2.15105711021124E-13,61.9999999999998,
0.));
#5776=CARTESIAN_POINT('',(-56.0000000000003,61.9999999999996,-6.85802207522519E-15));
#5777=CARTESIAN_POINT('',(-2.21963733096349E-13,61.9999999999997,56.0000000000002));
#5778=CARTESIAN_POINT('Origin',(-2.12675437930917E-13,61.9999999999997,
0.));
#5779=CARTESIAN_POINT('Origin',(-2.12675437930917E-13,61.9999999999997,
0.));
#5780=CARTESIAN_POINT('',(-2.2906916045395E-13,63.9999999999997,58.0000000000002));
#5781=CARTESIAN_POINT('Origin',(-2.22208662456179E-13,61.9999999999998,
58.0000000000002));
#5782=CARTESIAN_POINT('',(43.8178046004133,63.9999999999999,-38.));
#5783=CARTESIAN_POINT('Origin',(-2.19535935928689E-13,63.9999999999997,
0.));
#5784=CARTESIAN_POINT('',(41.1339720798706,62.0114315300489,-38.));
#5785=CARTESIAN_POINT('Ctrl Pts',(43.8178046004133,63.9999999999999,-38.));
#5786=CARTESIAN_POINT('Ctrl Pts',(43.4594642227257,63.9999999999999,-38.));
#5787=CARTESIAN_POINT('Ctrl Pts',(43.0349690410079,63.9313624698626,-38.));
#5788=CARTESIAN_POINT('Ctrl Pts',(42.398381143829,63.7105066153047,-38.));
#5789=CARTESIAN_POINT('Ctrl Pts',(42.0643495443749,63.5323654074303,-38.));
#5790=CARTESIAN_POINT('Ctrl Pts',(41.6188649978616,63.1625011801094,-38.));
#5791=CARTESIAN_POINT('Ctrl Pts',(41.4150926413892,62.9206514303181,-38.));
#5792=CARTESIAN_POINT('Ctrl Pts',(41.2006682164102,62.4874233680621,-38.));
#5793=CARTESIAN_POINT('Ctrl Pts',(41.1356921995111,62.232481043002,-38.));
#5794=CARTESIAN_POINT('Ctrl Pts',(41.1339720798706,62.0114315300489,-38.));
#5795=CARTESIAN_POINT('',(41.1339556851194,62.0090835271345,38.));
#5796=CARTESIAN_POINT('Ctrl Pts',(41.1339720798707,62.0114315300484,-38.));
#5797=CARTESIAN_POINT('Ctrl Pts',(41.5378675708182,62.011465189054,-37.5627943401587));
#5798=CARTESIAN_POINT('Ctrl Pts',(41.9345050198156,62.0114977099643,-37.1194669610288));
#5799=CARTESIAN_POINT('Ctrl Pts',(42.3240191945377,62.0115291274321,-36.6698939326639));
#5800=CARTESIAN_POINT('Ctrl Pts',(42.508108342725,62.0115439757104,-36.4574202379678));
#5801=CARTESIAN_POINT('Ctrl Pts',(42.6906058723339,62.0115585775212,-36.243550982485));
#5802=CARTESIAN_POINT('Ctrl Pts',(42.8715229676726,62.0115729365226,-36.028270407902));
#5803=CARTESIAN_POINT('Ctrl Pts',(43.1691570145251,62.0115965590979,-35.6741036084522));
#5804=CARTESIAN_POINT('Ctrl Pts',(43.4625105062847,62.0116195245126,-35.316113143293));
#5805=CARTESIAN_POINT('Ctrl Pts',(43.7511863459427,62.0116418174384,-34.95479206422));
#5806=CARTESIAN_POINT('Ctrl Pts',(44.0092631669743,62.011661747362,-34.6317702430334));
#5807=CARTESIAN_POINT('Ctrl Pts',(44.2636018952112,62.0116811398056,-34.3060870015161));
#5808=CARTESIAN_POINT('Ctrl Pts',(44.513946804719,62.011699983817,-33.9781160868287));
#5809=CARTESIAN_POINT('Ctrl Pts',(44.9124183662909,62.0117299776468,-33.4560879665742));
#5810=CARTESIAN_POINT('Ctrl Pts',(45.3007823806485,62.0117585820355,-32.9282686995972));
#5811=CARTESIAN_POINT('Ctrl Pts',(45.6791840228587,62.0117858374024,-32.3946914848435));
#5812=CARTESIAN_POINT('Ctrl Pts',(46.0592450736997,62.0118132122926,-31.8587743684177));
#5813=CARTESIAN_POINT('Ctrl Pts',(46.4292564142946,62.0118392263032,-31.3170484260819));
#5814=CARTESIAN_POINT('Ctrl Pts',(46.7893273274975,62.0118639203879,-30.7695107101662));
#5815=CARTESIAN_POINT('Ctrl Pts',(47.0250930021408,62.0118800894739,-30.4109963335472));
#5816=CARTESIAN_POINT('Ctrl Pts',(47.2565961247388,62.0118956926664,-30.0499895290226));
#5817=CARTESIAN_POINT('Ctrl Pts',(47.4838579530542,62.0119107414621,-29.686481875962));
#5818=CARTESIAN_POINT('Ctrl Pts',(47.8495677822757,62.0119349579904,-29.1015252085492));
#5819=CARTESIAN_POINT('Ctrl Pts',(48.204293167232,62.0119577388937,-28.5100992575856));
#5820=CARTESIAN_POINT('Ctrl Pts',(48.5480436433421,62.01197910361,-27.9122101670856));
#5821=CARTESIAN_POINT('Ctrl Pts',(48.6366313782987,62.0119846094987,-27.7581285178557));
#5822=CARTESIAN_POINT('Ctrl Pts',(48.7244899943061,62.0119900213324,-27.6036174841194));
#5823=CARTESIAN_POINT('Ctrl Pts',(48.8116191692164,62.0119953394441,-27.4486768895265));
#5824=CARTESIAN_POINT('Ctrl Pts',(49.2076260972417,62.0120195105561,-26.7444633014341));
#5825=CARTESIAN_POINT('Ctrl Pts',(49.5885686299212,62.0120417456002,-26.031376792441));
#5826=CARTESIAN_POINT('Ctrl Pts',(49.9542510971775,62.0120620654678,-25.3096201309785));
#5827=CARTESIAN_POINT('Ctrl Pts',(49.9812271085838,62.0120635644431,-25.2563769003739));
#5828=CARTESIAN_POINT('Ctrl Pts',(50.0081200547548,62.0120650529963,-25.2030864800111));
#5829=CARTESIAN_POINT('Ctrl Pts',(50.0349298464748,62.0120665311357,-25.1497489476434));
#5830=CARTESIAN_POINT('Ctrl Pts',(50.2703252167996,62.0120795094975,-24.681434672209));
#5831=CARTESIAN_POINT('Ctrl Pts',(50.4993133690921,62.0120916850446,-24.2094914308971));
#5832=CARTESIAN_POINT('Ctrl Pts',(50.7219802963322,62.0121030623635,-23.7336220668136));
#5833=CARTESIAN_POINT('Ctrl Pts',(50.868451137173,62.0121105463912,-23.4205940533962));
#5834=CARTESIAN_POINT('Ctrl Pts',(51.012185793409,62.0121176850223,-23.1058667532725));
#5835=CARTESIAN_POINT('Ctrl Pts',(51.1531972464791,62.0121244795624,-22.789351188351));
#5836=CARTESIAN_POINT('Ctrl Pts',(51.3210673250925,62.0121325682669,-22.4125485130439));
#5837=CARTESIAN_POINT('Ctrl Pts',(51.4850732756592,62.012140169318,-22.0332086150571));
#5838=CARTESIAN_POINT('Ctrl Pts',(51.6449228820795,62.0121472726493,-21.6519299860615));
#5839=CARTESIAN_POINT('Ctrl Pts',(51.8047054217536,62.0121543730003,-21.2708113269125));
#5840=CARTESIAN_POINT('Ctrl Pts',(51.9603350272497,62.0121609760492,-20.8877557340995));
#5841=CARTESIAN_POINT('Ctrl Pts',(52.1115677050986,62.0121670717421,-20.5033815847748));
#5842=CARTESIAN_POINT('Ctrl Pts',(52.1293310215895,62.0121677877231,-20.458234201534));
#5843=CARTESIAN_POINT('Ctrl Pts',(52.1470337325548,62.0121684967045,-20.4130686489935));
#5844=CARTESIAN_POINT('Ctrl Pts',(52.1646754866477,62.0121691986701,-20.3678859461551));
#5845=CARTESIAN_POINT('Ctrl Pts',(52.4827757330314,62.0121818558829,-19.5531920767413));
#5846=CARTESIAN_POINT('Ctrl Pts',(52.7810569708954,62.0121922321038,-18.7329183662393));
#5847=CARTESIAN_POINT('Ctrl Pts',(53.0594801179139,62.0122003722445,-17.9079797138351));
#5848=CARTESIAN_POINT('Ctrl Pts',(53.2654855976632,62.0122063951403,-17.2976070322818));
#5849=CARTESIAN_POINT('Ctrl Pts',(53.4606249872914,62.0122111938872,-16.6846825185638));
#5850=CARTESIAN_POINT('Ctrl Pts',(53.645006030693,62.0122147829815,-16.0691476324579));
#5851=CARTESIAN_POINT('Ctrl Pts',(53.7098220009675,62.0122160446656,-15.8527669777835));
#5852=CARTESIAN_POINT('Ctrl Pts',(53.7733080750946,62.0122171568666,-15.6360635542535));
#5853=CARTESIAN_POINT('Ctrl Pts',(53.8354675204326,62.0122181202142,-15.4190342371275));
#5854=CARTESIAN_POINT('Ctrl Pts',(54.0249493601744,62.0122210568053,-14.7574595711486));
#5855=CARTESIAN_POINT('Ctrl Pts',(54.2021067755319,62.0122226102135,-14.0928599079471));
#5856=CARTESIAN_POINT('Ctrl Pts',(54.3669672963198,62.0122227785237,-13.4252392951594));
#5857=CARTESIAN_POINT('Ctrl Pts',(54.5317686288195,62.0122229467735,-12.757858371783));
#5858=CARTESIAN_POINT('Ctrl Pts',(54.6842819835983,62.0122217309197,-12.0874582951485));
#5859=CARTESIAN_POINT('Ctrl Pts',(54.8244843840114,62.0122191290495,-11.4140305179011));
#5860=CARTESIAN_POINT('Ctrl Pts',(54.8978161216433,62.0122177681622,-11.0617995366224));
#5861=CARTESIAN_POINT('Ctrl Pts',(54.9677790714846,62.0122160280985,-10.7087400841896));
#5862=CARTESIAN_POINT('Ctrl Pts',(55.0343643255293,62.0122139085844,-10.3548500883884));
#5863=CARTESIAN_POINT('Ctrl Pts',(55.1738277395596,62.0122094692432,-9.61362430628843));
#5864=CARTESIAN_POINT('Ctrl Pts',(55.2984759194646,62.012203365266,-8.86875624929427));
#5865=CARTESIAN_POINT('Ctrl Pts',(55.4081555458839,62.0121955718983,-8.12037336202324));
#5866=CARTESIAN_POINT('Ctrl Pts',(55.4247934124446,62.0121943896823,-8.00684731328274));
#5867=CARTESIAN_POINT('Ctrl Pts',(55.4410867338072,62.012193168591,-7.89324038814436));
#5868=CARTESIAN_POINT('Ctrl Pts',(55.457034869806,62.012191908538,-7.77955303875739));
#5869=CARTESIAN_POINT('Ctrl Pts',(55.5175753408372,62.0121871252705,-7.34798625987619));
#5870=CARTESIAN_POINT('Ctrl Pts',(55.5731452267925,62.0121817805551,-6.91526060581588));
#5871=CARTESIAN_POINT('Ctrl Pts',(55.6237433222154,62.0121758616839,-6.48099760138376));
#5872=CARTESIAN_POINT('Ctrl Pts',(55.6634045101909,62.0121712221918,-6.14060165355911));
#5873=CARTESIAN_POINT('Ctrl Pts',(55.7000044146649,62.0121662299287,-5.79926035246736));
#5874=CARTESIAN_POINT('Ctrl Pts',(55.7334497888444,62.0121608936061,-5.45772072568573));
#5875=CARTESIAN_POINT('Ctrl Pts',(55.7426726331568,62.0121594220701,-5.36353828994967));
#5876=CARTESIAN_POINT('Ctrl Pts',(55.7516559017131,62.0121579243709,-5.26934080753018));
#5877=CARTESIAN_POINT('Ctrl Pts',(55.7603983329535,62.0121564006911,-5.1751440150118));
#5878=CARTESIAN_POINT('Ctrl Pts',(55.8175970056945,62.0121464317868,-4.55884731671826));
#5879=CARTESIAN_POINT('Ctrl Pts',(55.8644832568223,62.0121353507522,-3.94257835777548));
#5880=CARTESIAN_POINT('Ctrl Pts',(55.9011202625538,62.0121231749186,-3.32699092712286));
#5881=CARTESIAN_POINT('Ctrl Pts',(55.9162959151216,62.0121181314874,-3.07200445139562));
#5882=CARTESIAN_POINT('Ctrl Pts',(55.9297136672316,62.0121129002156,-2.81713486821982));
#5883=CARTESIAN_POINT('Ctrl Pts',(55.9413806163243,62.0121074823351,-2.56242840483791));
#5884=CARTESIAN_POINT('Ctrl Pts',(55.9687757179352,62.0120947606384,-1.9643535019748));
#5885=CARTESIAN_POINT('Ctrl Pts',(55.9865226639761,62.0120810100653,-1.36717903886914));
#5886=CARTESIAN_POINT('Ctrl Pts',(55.9947322782494,62.012066226294,-0.77073585089363));
#5887=CARTESIAN_POINT('Ctrl Pts',(55.998459676216,62.0120595140421,-0.499933709403522));
#5888=CARTESIAN_POINT('Ctrl Pts',(56.000220327323,62.012052588805,-0.229282197751845));
#5889=CARTESIAN_POINT('Ctrl Pts',(56.0000210920964,62.012045450178,0.0412349762717366));
#5890=CARTESIAN_POINT('Ctrl Pts',(55.9994875740913,62.0120263341508,0.765633896347442));
#5891=CARTESIAN_POINT('Ctrl Pts',(55.9849031765495,62.0120056879541,1.48906785379857));
#5892=CARTESIAN_POINT('Ctrl Pts',(55.9563530719782,62.0119834973098,2.2114637323107));
#5893=CARTESIAN_POINT('Ctrl Pts',(55.9507591585882,62.0119791494258,2.35300506949458));
#5894=CARTESIAN_POINT('Ctrl Pts',(55.9446289445313,62.0119747422508,2.49450657020774));
#5895=CARTESIAN_POINT('Ctrl Pts',(55.9379628370825,62.0119702756773,2.63596770169497));
#5896=CARTESIAN_POINT('Ctrl Pts',(55.9058777584782,62.0119487773196,3.31684354387251));
#5897=CARTESIAN_POINT('Ctrl Pts',(55.8613820941595,62.0119259029036,3.99678377855943));
#5898=CARTESIAN_POINT('Ctrl Pts',(55.8044873472033,62.0119016284166,4.67580561158339));
#5899=CARTESIAN_POINT('Ctrl Pts',(55.789231442081,62.0118951193926,4.85788028832961));
#5900=CARTESIAN_POINT('Ctrl Pts',(55.773083747807,62.0118885097029,5.03988891584848));
#5901=CARTESIAN_POINT('Ctrl Pts',(55.7560438508535,62.0118817988845,5.22183177609851));
#5902=CARTESIAN_POINT('Ctrl Pts',(55.6920225510572,62.0118565853918,5.90541680209062));
#5903=CARTESIAN_POINT('Ctrl Pts',(55.615410854639,62.0118299443551,6.58807330611238));
#5904=CARTESIAN_POINT('Ctrl Pts',(55.5261553576502,62.0118018392235,7.26979856450947));
#5905=CARTESIAN_POINT('Ctrl Pts',(55.5030591332503,62.011794566591,7.44620539745826));
#5906=CARTESIAN_POINT('Ctrl Pts',(55.4791160204489,62.0117871959234,7.62254982231334));
#5907=CARTESIAN_POINT('Ctrl Pts',(55.4543245380382,62.0117797265876,7.79883166888876));
#5908=CARTESIAN_POINT('Ctrl Pts',(55.3585683509376,62.011750876553,8.47971380427104));
#5909=CARTESIAN_POINT('Ctrl Pts',(55.2501595693073,62.0117205545226,9.15966304948901));
#5910=CARTESIAN_POINT('Ctrl Pts',(55.1289824351151,62.0116887132261,9.83865444210619));
#5911=CARTESIAN_POINT('Ctrl Pts',(55.0975453254334,62.0116804526055,10.0148058837531));
#5912=CARTESIAN_POINT('Ctrl Pts',(55.0652485912683,62.0116720897314,10.1908927684566));
#5913=CARTESIAN_POINT('Ctrl Pts',(55.032089672709,62.0116636237787,10.3669144595589));
#5914=CARTESIAN_POINT('Ctrl Pts',(54.9135687328307,62.0116333636639,10.9960741901775));
#5915=CARTESIAN_POINT('Ctrl Pts',(54.7840366361783,62.0116017866311,11.6244014107884));
#5916=CARTESIAN_POINT('Ctrl Pts',(54.6433306503092,62.0115688367575,12.25194527151));
#5917=CARTESIAN_POINT('Ctrl Pts',(54.5929324045582,62.0115570347306,12.4767197153037));
#5918=CARTESIAN_POINT('Ctrl Pts',(54.5411001729428,62.0115450565767,12.7013934683708));
#5919=CARTESIAN_POINT('Ctrl Pts',(54.4878249957722,62.011532899726,12.9259681060992));
#5920=CARTESIAN_POINT('Ctrl Pts',(54.4137006342804,62.0115159853046,13.2384297911268));
#5921=CARTESIAN_POINT('Ctrl Pts',(54.3367784741253,62.0114987249528,13.5506990328332));
#5922=CARTESIAN_POINT('Ctrl Pts',(54.2572438873394,62.0114811570873,13.8620047849093));
#5923=CARTESIAN_POINT('Ctrl Pts',(54.2283995452362,62.0114747858526,13.9749042161435));
#5924=CARTESIAN_POINT('Ctrl Pts',(54.1992120853552,62.0114683741721,14.0876770418473));
#5925=CARTESIAN_POINT('Ctrl Pts',(54.1696919905561,62.0114619238783,14.2002869055221));
#5926=CARTESIAN_POINT('Ctrl Pts',(54.0587740072792,62.0114376877235,14.6234040757373));
#5927=CARTESIAN_POINT('Ctrl Pts',(53.9431637590319,62.0114129064316,15.0442218079722));
#5928=CARTESIAN_POINT('Ctrl Pts',(53.8228416772755,62.0113875607373,15.4630315513008));
#5929=CARTESIAN_POINT('Ctrl Pts',(53.6191496499546,62.0113446532697,16.1720303022786));
#5930=CARTESIAN_POINT('Ctrl Pts',(53.4019500394013,62.011300128295,16.8752731946603));
#5931=CARTESIAN_POINT('Ctrl Pts',(53.1714548723221,62.0112539514119,17.5727042036621));
#5932=CARTESIAN_POINT('Ctrl Pts',(53.1296403304496,62.0112455743807,17.6992264145119));
#5933=CARTESIAN_POINT('Ctrl Pts',(53.0873880903754,62.0112371429847,17.8255573514516));
#5934=CARTESIAN_POINT('Ctrl Pts',(53.044699235177,62.0112286570187,17.9516966717651));
#5935=CARTESIAN_POINT('Ctrl Pts',(52.8304155607197,62.0111860603276,18.5848735729654));
#5936=CARTESIAN_POINT('Ctrl Pts',(52.6051347514235,62.0111420886329,19.2132228618125));
#5937=CARTESIAN_POINT('Ctrl Pts',(52.3689251517624,62.0110966991285,19.836812402838));
#5938=CARTESIAN_POINT('Ctrl Pts',(52.298685369297,62.0110832020101,20.0222442979523));
#5939=CARTESIAN_POINT('Ctrl Pts',(52.227478875668,62.0110695795231,20.2072552362763));
#5940=CARTESIAN_POINT('Ctrl Pts',(52.1553066088181,62.0110558305417,20.3918467787042));
#5941=CARTESIAN_POINT('Ctrl Pts',(51.8999966385941,62.0110071934105,21.0448408338706));
#5942=CARTESIAN_POINT('Ctrl Pts',(51.6326051540701,62.0109569733346,21.6925867841522));
#5943=CARTESIAN_POINT('Ctrl Pts',(51.3531674886488,62.0109051010724,22.3350737339108));
#5944=CARTESIAN_POINT('Ctrl Pts',(51.0738152139627,62.0108532446614,22.9773643521084));
#5945=CARTESIAN_POINT('Ctrl Pts',(50.7824239594258,62.0107997370736,23.6143995446689));
#5946=CARTESIAN_POINT('Ctrl Pts',(50.4789812557923,62.0107445091308,24.2461478145941));
#5947=CARTESIAN_POINT('Ctrl Pts',(50.3372425961395,62.0107187120545,24.5412386239791));
#5948=CARTESIAN_POINT('Ctrl Pts',(50.1928738366941,62.0106925396239,24.8351755838836));
#5949=CARTESIAN_POINT('Ctrl Pts',(50.0458702895881,62.0106659847888,25.127953604534));
#5950=CARTESIAN_POINT('Ctrl Pts',(49.7551858170679,62.0106134753197,25.706892182369));
#5951=CARTESIAN_POINT('Ctrl Pts',(49.4542054026347,62.0105594706101,26.2812943293165));
#5952=CARTESIAN_POINT('Ctrl Pts',(49.1428195444775,62.0105038711921,26.8511894802682));
#5953=CARTESIAN_POINT('Ctrl Pts',(48.8330311455835,62.010448557008,27.4181609779323));
#5954=CARTESIAN_POINT('Ctrl Pts',(48.5129435967346,62.0103916644357,27.9806718822024));
#5955=CARTESIAN_POINT('Ctrl Pts',(48.1824079257721,62.0103330955301,28.5387202958513));
#5956=CARTESIAN_POINT('Ctrl Pts',(47.9576449716585,62.010293268905,28.9181910187081));
#5957=CARTESIAN_POINT('Ctrl Pts',(47.7280500113292,62.0102526671523,29.2955976696472));
#5958=CARTESIAN_POINT('Ctrl Pts',(47.49356595267,62.0102112594757,29.670930431553));
#5959=CARTESIAN_POINT('Ctrl Pts',(47.2620846493753,62.0101703820573,30.0414567581269));
#5960=CARTESIAN_POINT('Ctrl Pts',(47.0258323928037,62.0101287192237,30.4099606921261));
#5961=CARTESIAN_POINT('Ctrl Pts',(46.7851812262161,62.0100863113628,30.7757967597325));
#5962=CARTESIAN_POINT('Ctrl Pts',(46.5445300596285,62.010043903502,31.141632827339));
#5963=CARTESIAN_POINT('Ctrl Pts',(46.2994801027285,62.0100007506138,31.5048008283505));
#5964=CARTESIAN_POINT('Ctrl Pts',(46.0504549827791,62.0099568930863,31.8646884781416));
#5965=CARTESIAN_POINT('Ctrl Pts',(45.7176003038583,62.0098982717583,32.3457254439829));
#5966=CARTESIAN_POINT('Ctrl Pts',(45.3776535651338,62.0098383915342,32.8209111895306));
#5967=CARTESIAN_POINT('Ctrl Pts',(45.0305386446111,62.009777170325,33.2904380565692));
#5968=CARTESIAN_POINT('Ctrl Pts',(44.8582657349873,62.0097467862786,33.5234639357492));
#5969=CARTESIAN_POINT('Ctrl Pts',(44.6842265206803,62.0097160719302,33.7550955348643));
#5970=CARTESIAN_POINT('Ctrl Pts',(44.5084077393491,62.0096850172446,33.9853537117308));
#5971=CARTESIAN_POINT('Ctrl Pts',(44.0783183399654,62.0096090510086,34.5486132238367));
#5972=CARTESIAN_POINT('Ctrl Pts',(43.6375851668711,62.0095310482173,35.1036522194153));
#5973=CARTESIAN_POINT('Ctrl Pts',(43.1862189041955,62.0094508349908,35.6504277348031));
#5974=CARTESIAN_POINT('Ctrl Pts',(42.7359482888616,62.0093708164741,36.1958760062442));
#5975=CARTESIAN_POINT('Ctrl Pts',(42.2750958715132,62.0092885982405,36.7331011603559));
#5976=CARTESIAN_POINT('Ctrl Pts',(41.8036345689526,62.009204007673,37.2620250230665));
#5977=CARTESIAN_POINT('Ctrl Pts',(41.582739475743,62.009164374216,37.5098432115788));
#5978=CARTESIAN_POINT('Ctrl Pts',(41.3595149744804,62.0091242199772,37.7558385404457));
#5979=CARTESIAN_POINT('Ctrl Pts',(41.1339556851197,62.0090835272022,38.0000000000002));
#5980=CARTESIAN_POINT('',(43.8178046004133,63.9999999999999,38.));
#5981=CARTESIAN_POINT('Ctrl Pts',(41.1339556851194,62.0090835271345,38.));
#5982=CARTESIAN_POINT('Ctrl Pts',(41.1353258249379,62.2306725157175,38.));
#5983=CARTESIAN_POINT('Ctrl Pts',(41.2003227396635,62.4867253588613,38.));
#5984=CARTESIAN_POINT('Ctrl Pts',(41.4150926413892,62.9206514303181,38.));
#5985=CARTESIAN_POINT('Ctrl Pts',(41.6188649978616,63.1625011801094,38.));
#5986=CARTESIAN_POINT('Ctrl Pts',(42.0643495443749,63.5323654074303,38.));
#5987=CARTESIAN_POINT('Ctrl Pts',(42.398381143829,63.7105066153047,38.));
#5988=CARTESIAN_POINT('Ctrl Pts',(43.0349690410079,63.9313624698626,38.));
#5989=CARTESIAN_POINT('Ctrl Pts',(43.4594642227257,63.9999999999999,38.));
#5990=CARTESIAN_POINT('Ctrl Pts',(43.8178046004133,63.9999999999999,38.));
#5991=CARTESIAN_POINT('Origin',(-2.19535935928689E-13,63.9999999999997,
0.));
#5992=CARTESIAN_POINT('Origin',(88.,64.0000000000001,0.));
#5993=CARTESIAN_POINT('',(59.464274989274,64.,-38.));
#5994=CARTESIAN_POINT('Origin',(59.464274989274,64.,-8.));
#5995=CARTESIAN_POINT('',(43.8178046004133,63.9999999999999,-38.));
#5996=CARTESIAN_POINT('',(59.464274989274,64.,38.));
#5997=CARTESIAN_POINT('',(59.464274989274,64.,38.));
#5998=CARTESIAN_POINT('Origin',(59.464274989274,64.,8.));
#5999=CARTESIAN_POINT('',(-5.9999999999995,63.9999999999997,70.0000000000003));
#6000=CARTESIAN_POINT('Origin',(5.13675145228373E-13,63.9999999999998,70.0000000000002));
#6001=CARTESIAN_POINT('',(-70.0000000000004,63.9999999999995,-6.00000000000001));
#6002=CARTESIAN_POINT('Origin',(-70.0000000000004,63.9999999999995,0.));
#6003=CARTESIAN_POINT('',(5.99999999999955,63.9999999999998,-70.0000000000002));
#6004=CARTESIAN_POINT('Origin',(-4.63939629647707E-13,63.9999999999998,
-70.0000000000002));
#6005=CARTESIAN_POINT('Origin',(30.,-1.01376661467639E-14,0.));
#6006=CARTESIAN_POINT('',(-4.40872847693047E-15,-1.11022302462516E-13,36.));
#6007=CARTESIAN_POINT('Origin',(0.,-1.11022302462516E-13,0.));
#6008=CARTESIAN_POINT('',(30.,-8.11483249594263E-15,0.));
#6009=CARTESIAN_POINT('Origin',(0.,-1.11022302462516E-13,0.));
#6010=CARTESIAN_POINT('Origin',(0.,-1.11022302462516E-13,0.));
#6011=CARTESIAN_POINT('',(26.,-4.00000000000002,0.));
#6012=CARTESIAN_POINT('',(-25.9999999999999,-4.0000000000002,-3.18408167778311E-15));
#6013=CARTESIAN_POINT('Origin',(1.37209959955428E-14,-4.00000000000011,
0.));
#6014=CARTESIAN_POINT('Origin',(1.37209959955428E-14,-4.00000000000011,
0.));
#6015=CARTESIAN_POINT('',(30.,-8.11483249594263E-15,-3.67394039744206E-15));
#6016=CARTESIAN_POINT('Origin',(2.26992721413867E-12,-661.73832129271,0.));
#6017=CARTESIAN_POINT('',(-25.9999999999999,-30.0000000000003,-3.18408167778311E-15));
#6018=CARTESIAN_POINT('',(-25.9999999999977,-661.73832129271,-3.18408167778311E-15));
#6019=CARTESIAN_POINT('Origin',(1.02907469966573E-13,-30.0000000000001,
0.));
#6020=CARTESIAN_POINT('Origin',(26.,-30.,0.));
#6021=CARTESIAN_POINT('',(-23.9999999999997,-30.0000000000002,-2.93915231795363E-15));
#6022=CARTESIAN_POINT('Origin',(1.02907469966573E-13,-30.0000000000001,
0.));
#6023=CARTESIAN_POINT('Origin',(2.26992721413867E-12,-661.73832129271,0.));
#6024=CARTESIAN_POINT('',(-23.9999999999995,-80.0000000000003,-2.93915231795363E-15));
#6025=CARTESIAN_POINT('',(-23.9999999999975,-661.73832129271,-2.93915231795363E-15));
#6026=CARTESIAN_POINT('Origin',(2.74419919910861E-13,-80.0000000000001,
0.));
#6027=CARTESIAN_POINT('Origin',(24.,-80.0000000000001,0.));
#6028=CARTESIAN_POINT('',(-83.9999999999995,-80.0000000000005,-1.02870331128377E-14));
#6029=CARTESIAN_POINT('Origin',(2.74419919910862E-13,-80.0000000000003,
0.));
#6030=CARTESIAN_POINT('',(-71.9999999999997,-80.0000000000005,2.22475088246643E-13));
#6031=CARTESIAN_POINT('Origin',(-63.9999999999997,-80.0000000000004,2.23454805685961E-13));
#6032=CARTESIAN_POINT('',(-7.99999999999973,-80.0000000000002,64.));
#6033=CARTESIAN_POINT('Origin',(2.74419919910862E-13,-80.0000000000002,
64.));
#6034=CARTESIAN_POINT('',(56.0000000000003,-80.,-6.71344134497199E-13));
#6035=CARTESIAN_POINT('Origin',(64.0000000000003,-80.,-6.70364417057882E-13));
#6036=CARTESIAN_POINT('',(-7.99999999999973,-80.0000000000002,-64.));
#6037=CARTESIAN_POINT('Origin',(2.74419919910862E-13,-80.0000000000002,
-64.));
#6038=CARTESIAN_POINT('Origin',(2.26992721413867E-12,-661.73832129271,0.));
#6039=CARTESIAN_POINT('',(-83.9999999999995,-65.0000000000006,0.));
#6040=CARTESIAN_POINT('',(-83.9999999999975,-661.73832129271,-1.02870331128377E-14));
#6041=CARTESIAN_POINT('',(2.12679151814737E-13,-65.0000000000003,-83.9999999999998));
#6042=CARTESIAN_POINT('Origin',(2.22966184927575E-13,-65.0000000000003,
0.));
#6043=CARTESIAN_POINT('Origin',(2.22966184927575E-13,-65.0000000000003,
0.));
#6044=CARTESIAN_POINT('Origin',(84.,-63.9999999999999,0.));
#6045=CARTESIAN_POINT('',(2.09371367495766E-13,-64.0000000000002,-82.9999999999998));
#6046=CARTESIAN_POINT('Origin',(2.19535935928689E-13,-64.0000000000002,
0.));
#6047=CARTESIAN_POINT('',(-71.9999999999998,-64.0000000000005,2.23454805685961E-13));
#6048=CARTESIAN_POINT('Origin',(-63.9999999999998,-64.0000000000005,2.23454805685961E-13));
#6049=CARTESIAN_POINT('',(-7.99999999999978,-64.0000000000003,64.));
#6050=CARTESIAN_POINT('Origin',(2.1953593592869E-13,-64.0000000000002,64.));
#6051=CARTESIAN_POINT('',(56.0000000000002,-64.,-6.70364417057882E-13));
#6052=CARTESIAN_POINT('Origin',(64.0000000000002,-64.,-6.70364417057882E-13));
#6053=CARTESIAN_POINT('',(-7.99999999999978,-64.0000000000003,-64.));
#6054=CARTESIAN_POINT('Origin',(2.1953593592869E-13,-64.0000000000002,-64.));
#6055=CARTESIAN_POINT('',(-39.9999999999996,-64.0000000000002,-4.89858719658939E-15));
#6056=CARTESIAN_POINT('Origin',(2.19535935928689E-13,-64.0000000000001,
0.));
#6057=CARTESIAN_POINT('Origin',(2.26992721413867E-12,-661.73832129271,0.));
#6058=CARTESIAN_POINT('',(-39.9999999999998,-20.0000000000003,-4.89858719658939E-15));
#6059=CARTESIAN_POINT('',(-39.9999999999976,-661.73832129271,-4.89858719658939E-15));
#6060=CARTESIAN_POINT('',(6.44903518424829E-14,-20.0000000000001,39.9999999999999));
#6061=CARTESIAN_POINT('Origin',(6.86049799777153E-14,-20.0000000000001,
0.));
#6062=CARTESIAN_POINT('Origin',(6.86049799777153E-14,-20.0000000000001,
0.));
#6063=CARTESIAN_POINT('Origin',(6.93889390390723E-14,-20.0000000000001,
0.));
#6064=CARTESIAN_POINT('',(5.73849244848819E-14,-18.0000000000001,42.));
#6065=CARTESIAN_POINT('Origin',(6.42454224826534E-14,-20.0000000000001,
41.9999999999999));
#6066=CARTESIAN_POINT('Origin',(6.17444819799439E-14,-18.0000000000001,
0.));
#6067=CARTESIAN_POINT('Origin',(42.,-18.,0.));
#6068=CARTESIAN_POINT('',(5.6258156874715E-14,-18.0000000000001,47.9999999999999));
#6069=CARTESIAN_POINT('Origin',(6.17444819799439E-14,-18.0000000000001,
0.));
#6070=CARTESIAN_POINT('Origin',(3.46944695195361E-14,-10.0000000000001,
0.));
#6071=CARTESIAN_POINT('',(2.78364474443114E-14,-10.0000000000002,56.));
#6072=CARTESIAN_POINT('Origin',(2.88161648836289E-14,-10.0000000000001,
48.));
#6073=CARTESIAN_POINT('',(-56.0000000000001,-10.0000000000007,-6.85802207522519E-15));
#6074=CARTESIAN_POINT('Origin',(3.43024899888579E-14,-10.0000000000002,
0.));
#6075=CARTESIAN_POINT('Origin',(3.43024899888579E-14,-10.0000000000002,
0.));
#6076=CARTESIAN_POINT('Origin',(3.43024899888579E-14,-10.0000000000002,
0.));
#6077=CARTESIAN_POINT('Origin',(2.26992721413867E-12,-661.73832129271,0.));
#6078=CARTESIAN_POINT('',(-55.9999999999978,-661.73832129271,-6.85802207522519E-15));
#6079=CARTESIAN_POINT('Origin',(2.26992721413867E-12,-661.73832129271,0.));
#6080=CARTESIAN_POINT('',(89.1964124839111,65.9999999999999,-12.));
#6081=CARTESIAN_POINT('',(-90.0000000000005,79.9999999999994,-1.10218211923262E-14));
#6082=CARTESIAN_POINT('',(-89.999999999998,-661.73832129271,-1.10218211923262E-14));
#6083=CARTESIAN_POINT('Origin',(-2.74419919910861E-13,79.9999999999996,
0.));
#6084=CARTESIAN_POINT('',(89.1964124839111,65.9999999999999,12.));
#6085=CARTESIAN_POINT('Origin',(39.9999999999977,79.9999999999999,0.));
#6086=CARTESIAN_POINT('',(-2.79440971787365E-13,79.9999999999998,-40.999999999998));
#6087=CARTESIAN_POINT('Origin',(-2.74419919910861E-13,79.9999999999998,
0.));
#6088=CARTESIAN_POINT('',(-5.99999999999955,79.9999999999997,70.0000000000003));
#6089=CARTESIAN_POINT('Origin',(4.58791161246202E-13,79.9999999999997,70.0000000000003));
#6090=CARTESIAN_POINT('',(-70.0000000000005,79.9999999999995,-6.00000000000001));
#6091=CARTESIAN_POINT('Origin',(-70.0000000000006,79.9999999999994,0.));
#6092=CARTESIAN_POINT('',(5.99999999999949,79.9999999999997,-70.0000000000003));
#6093=CARTESIAN_POINT('Origin',(-5.1882361362988E-13,79.9999999999997,-70.0000000000003));
#6094=CARTESIAN_POINT('',(70.,79.9999999999999,6.00000000000001));
#6095=CARTESIAN_POINT('Origin',(70.,79.9999999999999,0.));
#6096=CARTESIAN_POINT('Origin',(2.26992721413867E-12,-661.73832129271,0.));
#6097=CARTESIAN_POINT('',(-39.9999999999983,78.9999999999997,0.));
#6098=CARTESIAN_POINT('',(-2.75888258108565E-13,78.9999999999998,-39.999999999998));
#6099=CARTESIAN_POINT('Origin',(-2.70989670911976E-13,78.9999999999998,
0.));
#6100=CARTESIAN_POINT('Origin',(-2.70989670911976E-13,78.9999999999998,
0.));
#6101=CARTESIAN_POINT('',(-39.9999999999982,71.9999999999997,-4.89858719658917E-15));
#6102=CARTESIAN_POINT('',(-39.9999999999957,-661.73832129271,-4.89858719658917E-15));
#6103=CARTESIAN_POINT('Origin',(-2.46977927919775E-13,71.9999999999998,
0.));
#6104=CARTESIAN_POINT('Origin',(44.,72.,0.));
#6105=CARTESIAN_POINT('',(-44.0000000000004,71.9999999999997,-5.38844591624837E-15));
#6106=CARTESIAN_POINT('Origin',(-2.46977927919775E-13,71.9999999999998,
0.));
#6107=CARTESIAN_POINT('Origin',(2.26992721413867E-12,-661.73832129271,0.));
#6108=CARTESIAN_POINT('',(-44.0000000000001,-2.50000000000014,-5.38844591624837E-15));
#6109=CARTESIAN_POINT('',(-43.9999999999978,-661.73832129271,-5.38844591624837E-15));
#6110=CARTESIAN_POINT('Origin',(8.57562249721397E-15,-2.50000000000006,
0.));
#6111=CARTESIAN_POINT('',(36.8781778291716,21.9999999999997,-24.));
#6112=CARTESIAN_POINT('',(36.8781778291716,21.9999999999997,24.));
#6113=CARTESIAN_POINT('Ctrl Pts',(36.8781778291716,21.9999999999997,-24.));
#6114=CARTESIAN_POINT('Ctrl Pts',(36.8781778291716,23.547692417105,-24.));
#6115=CARTESIAN_POINT('Ctrl Pts',(36.9785122566031,25.1334863360913,-23.8479816802424));
#6116=CARTESIAN_POINT('Ctrl Pts',(37.3739040154025,28.2623534606261,-23.2234342163971));
#6117=CARTESIAN_POINT('Ctrl Pts',(37.668184781229,29.8055820781137,-22.7511923092776));
#6118=CARTESIAN_POINT('Ctrl Pts',(38.3858791967795,32.7476022190956,-21.5182029027182));
#6119=CARTESIAN_POINT('Ctrl Pts',(38.8088904227423,34.1493429299749,-20.7564665668354));
#6120=CARTESIAN_POINT('Ctrl Pts',(39.6947646020434,36.7360406873461,-19.0075391135467));
#6121=CARTESIAN_POINT('Ctrl Pts',(40.1568366987602,37.9210704450902,-18.0200550518638));
#6122=CARTESIAN_POINT('Ctrl Pts',(41.0325054029201,40.0157721605676,-15.9253533363863));
#6123=CARTESIAN_POINT('Ctrl Pts',(41.4789748531813,41.0026054632418,-14.7424846218932));
#6124=CARTESIAN_POINT('Ctrl Pts',(42.3095898911624,42.7531938862499,-12.1550323282439));
#6125=CARTESIAN_POINT('Ctrl Pts',(42.6931404535345,43.5170818808236,-10.7503476715086));
#6126=CARTESIAN_POINT('Ctrl Pts',(43.3290028514715,44.7526497513758,-7.8020338794679));
#6127=CARTESIAN_POINT('Ctrl Pts',(43.5814918372967,45.2253213499122,-6.25551064938976));
#6128=CARTESIAN_POINT('Ctrl Pts',(43.9170909199956,45.8491089125422,-3.1252150936039));
#6129=CARTESIAN_POINT('Ctrl Pts',(44.,45.9999999999997,-1.54137641234701));
#6130=CARTESIAN_POINT('Ctrl Pts',(44.,45.9999999999997,1.54137641234701));
#6131=CARTESIAN_POINT('Ctrl Pts',(43.9170909199956,45.8491089125422,3.1252150936039));
#6132=CARTESIAN_POINT('Ctrl Pts',(43.5814918372967,45.2253213499122,6.25551064938976));
#6133=CARTESIAN_POINT('Ctrl Pts',(43.3290028514715,44.7526497513758,7.8020338794679));
#6134=CARTESIAN_POINT('Ctrl Pts',(42.6931404535345,43.5170818808236,10.7503476715086));
#6135=CARTESIAN_POINT('Ctrl Pts',(42.3095898911624,42.7531938862499,12.1550323282439));
#6136=CARTESIAN_POINT('Ctrl Pts',(41.4789748531813,41.0026054632418,14.7424846218932));
#6137=CARTESIAN_POINT('Ctrl Pts',(41.0325054029201,40.0157721605676,15.9253533363863));
#6138=CARTESIAN_POINT('Ctrl Pts',(40.1568366987602,37.9210704450902,18.0200550518638));
#6139=CARTESIAN_POINT('Ctrl Pts',(39.6947646020433,36.7360406873461,19.0075391135467));
#6140=CARTESIAN_POINT('Ctrl Pts',(38.8088904227423,34.1493429299749,20.7564665668354));
#6141=CARTESIAN_POINT('Ctrl Pts',(38.3858791967795,32.7476022190956,21.5182029027182));
#6142=CARTESIAN_POINT('Ctrl Pts',(37.668184781229,29.8055820781137,22.7511923092776));
#6143=CARTESIAN_POINT('Ctrl Pts',(37.3739040154025,28.2623534606261,23.2234342163971));
#6144=CARTESIAN_POINT('Ctrl Pts',(36.9785122566031,25.1334863360913,23.8479816802424));
#6145=CARTESIAN_POINT('Ctrl Pts',(36.8781778291716,23.547692417105,24.));
#6146=CARTESIAN_POINT('Ctrl Pts',(36.8781778291716,21.9999999999997,24.));
#6147=CARTESIAN_POINT('Ctrl Pts',(36.8781778291716,21.9999999999997,24.));
#6148=CARTESIAN_POINT('Ctrl Pts',(36.8781778291716,20.4523075828945,24.));
#6149=CARTESIAN_POINT('Ctrl Pts',(36.9785122566031,18.8665136639082,23.8479816802424));
#6150=CARTESIAN_POINT('Ctrl Pts',(37.3739040154025,15.7376465393734,23.2234342163972));
#6151=CARTESIAN_POINT('Ctrl Pts',(37.6681847812291,14.1944179218858,22.7511923092776));
#6152=CARTESIAN_POINT('Ctrl Pts',(38.3858791967795,11.2523977809039,21.5182029027182));
#6153=CARTESIAN_POINT('Ctrl Pts',(38.8088904227423,9.85065707002456,20.7564665668354));
#6154=CARTESIAN_POINT('Ctrl Pts',(39.6947646020434,7.26395931265332,19.0075391135467));
#6155=CARTESIAN_POINT('Ctrl Pts',(40.1568366987603,6.07892955490932,18.0200550518638));
#6156=CARTESIAN_POINT('Ctrl Pts',(41.0325054029202,3.98422783943184,15.9253533363864));
#6157=CARTESIAN_POINT('Ctrl Pts',(41.4789748531814,2.99739453675761,14.7424846218932));
#6158=CARTESIAN_POINT('Ctrl Pts',(42.3095898911626,1.24680611374955,12.1550323282439));
#6159=CARTESIAN_POINT('Ctrl Pts',(42.6931404535346,0.482918119175804,10.7503476715086));
#6160=CARTESIAN_POINT('Ctrl Pts',(43.3290028514716,-0.752649751376416,7.8020338794679));
#6161=CARTESIAN_POINT('Ctrl Pts',(43.5814918372968,-1.22532134991275,6.25551064938977));
#6162=CARTESIAN_POINT('Ctrl Pts',(43.9170909199958,-1.84910891254281,3.12521509360391));
#6163=CARTESIAN_POINT('Ctrl Pts',(44.0000000000001,-2.00000000000031,1.54137641234701));
#6164=CARTESIAN_POINT('Ctrl Pts',(44.0000000000001,-2.00000000000031,-1.54137641234702));
#6165=CARTESIAN_POINT('Ctrl Pts',(43.9170909199958,-1.84910891254281,-3.12521509360392));
#6166=CARTESIAN_POINT('Ctrl Pts',(43.5814918372968,-1.22532134991275,-6.25551064938977));
#6167=CARTESIAN_POINT('Ctrl Pts',(43.3290028514716,-0.752649751376415,-7.8020338794679));
#6168=CARTESIAN_POINT('Ctrl Pts',(42.6931404535346,0.482918119175804,-10.7503476715086));
#6169=CARTESIAN_POINT('Ctrl Pts',(42.3095898911626,1.24680611374955,-12.1550323282439));
#6170=CARTESIAN_POINT('Ctrl Pts',(41.4789748531814,2.99739453675761,-14.7424846218932));
#6171=CARTESIAN_POINT('Ctrl Pts',(41.0325054029202,3.98422783943184,-15.9253533363864));
#6172=CARTESIAN_POINT('Ctrl Pts',(40.1568366987603,6.07892955490932,-18.0200550518638));
#6173=CARTESIAN_POINT('Ctrl Pts',(39.6947646020434,7.26395931265332,-19.0075391135467));
#6174=CARTESIAN_POINT('Ctrl Pts',(38.8088904227423,9.85065707002456,-20.7564665668354));
#6175=CARTESIAN_POINT('Ctrl Pts',(38.3858791967795,11.2523977809039,-21.5182029027182));
#6176=CARTESIAN_POINT('Ctrl Pts',(37.6681847812291,14.1944179218858,-22.7511923092776));
#6177=CARTESIAN_POINT('Ctrl Pts',(37.3739040154025,15.7376465393734,-23.2234342163972));
#6178=CARTESIAN_POINT('Ctrl Pts',(36.9785122566031,18.8665136639082,-23.8479816802424));
#6179=CARTESIAN_POINT('Ctrl Pts',(36.8781778291716,20.4523075828945,-24.));
#6180=CARTESIAN_POINT('Ctrl Pts',(36.8781778291716,21.9999999999997,-24.));
#6181=CARTESIAN_POINT('Origin',(38.5,-2.50000000000001,0.));
#6182=CARTESIAN_POINT('',(3.86073232049693E-15,-2.50000000000006,38.5));
#6183=CARTESIAN_POINT('Origin',(8.57562249721397E-15,-2.50000000000006,
0.));
#6184=CARTESIAN_POINT('Origin',(0.,-1.11022302462516E-13,0.));
#6185=CARTESIAN_POINT('Origin',(-4.71489017671731E-15,-1.11022302462516E-13,
38.5));
#6186=CARTESIAN_POINT('Origin',(114.,21.9999999999997,0.));
#6187=CARTESIAN_POINT('',(130.,21.9999999999997,84.));
#6188=CARTESIAN_POINT('Origin',(130.,21.9999999999997,0.));
#6189=CARTESIAN_POINT('',(114.,21.9999999999997,84.));
#6190=CARTESIAN_POINT('',(114.,21.9999999999997,84.));
#6191=CARTESIAN_POINT('Origin',(114.,21.9999999999997,0.));
#6192=CARTESIAN_POINT('Origin',(114.,21.9999999999997,0.));
#6193=CARTESIAN_POINT('',(114.,21.9999999999995,-56.));
#6194=CARTESIAN_POINT('Origin',(114.,21.9999999999995,-64.));
#6195=CARTESIAN_POINT('',(114.,-42.0000000000003,8.));
#6196=CARTESIAN_POINT('Origin',(114.,-42.0000000000003,0.));
#6197=CARTESIAN_POINT('',(114.,22.0000000000004,72.));
#6198=CARTESIAN_POINT('Origin',(114.,22.0000000000004,64.));
#6199=CARTESIAN_POINT('',(114.,85.9999999999997,8.));
#6200=CARTESIAN_POINT('Origin',(114.,85.9999999999997,0.));
#6201=CARTESIAN_POINT('Origin',(130.,21.9999999999997,0.));
#6202=CARTESIAN_POINT('',(130.,21.9999999999995,-56.));
#6203=CARTESIAN_POINT('Origin',(130.,21.9999999999995,-64.));
#6204=CARTESIAN_POINT('',(130.,-42.0000000000003,8.));
#6205=CARTESIAN_POINT('Origin',(130.,-42.0000000000003,0.));
#6206=CARTESIAN_POINT('',(130.,22.0000000000004,72.));
#6207=CARTESIAN_POINT('Origin',(130.,22.0000000000004,64.));
#6208=CARTESIAN_POINT('',(130.,85.9999999999997,8.));
#6209=CARTESIAN_POINT('Origin',(130.,85.9999999999997,0.));
#6210=CARTESIAN_POINT('',(130.,21.9999999999997,24.));
#6211=CARTESIAN_POINT('Origin',(130.,21.9999999999997,0.));
#6212=CARTESIAN_POINT('Origin',(3.62800908907132E-5,21.9999999999997,-8.87342752119391E-6));
#6213=CARTESIAN_POINT('',(41.13395568512,21.9999999999999,38.));
#6214=CARTESIAN_POINT('',(41.1339720798708,21.9999999999999,-38.));
#6215=CARTESIAN_POINT('Origin',(41.1339720798708,21.9999999999999,-38.));
#6216=CARTESIAN_POINT('',(59.4642749892742,22.,-38.));
#6217=CARTESIAN_POINT('Origin',(81.5843122174847,22.,38.));
#6218=CARTESIAN_POINT('',(59.4642749892742,22.,38.));
#6219=CARTESIAN_POINT('Origin',(-90.0010000000005,21.9999999999997,0.));
#6220=CARTESIAN_POINT('',(-90.0010000000005,21.9999999999997,24.));
#6221=CARTESIAN_POINT('Origin',(91.3725830020305,85.9999999999997,0.));
#6222=CARTESIAN_POINT('',(91.3725830020305,85.9999999999997,8.));
#6223=CARTESIAN_POINT('Origin',(91.3725830020305,22.0000000000004,64.));
#6224=CARTESIAN_POINT('',(91.3725830020305,22.0000000000004,72.));
#6225=CARTESIAN_POINT('Origin',(91.3725830020305,-42.0000000000003,0.));
#6226=CARTESIAN_POINT('',(91.3725830020305,-42.0000000000003,8.));
#6227=CARTESIAN_POINT('Origin',(91.3725830020305,21.9999999999995,-64.));
#6228=CARTESIAN_POINT('',(91.3725830020305,21.9999999999995,-56.));
#6229=CARTESIAN_POINT('Origin',(1.41918261424034E-13,-41.3725830020307,
-64.));
#6230=CARTESIAN_POINT('',(-7.99999999999986,-41.3725830020308,-64.));
#6231=CARTESIAN_POINT('Origin',(64.0000000000001,-41.3725830020305,-6.70364417057882E-13));
#6232=CARTESIAN_POINT('',(56.0000000000001,-41.3725830020305,-6.71344134497199E-13));
#6233=CARTESIAN_POINT('Origin',(1.41918261424034E-13,-41.3725830020307,
64.));
#6234=CARTESIAN_POINT('',(-7.99999999999986,-41.3725830020307,64.));
#6235=CARTESIAN_POINT('Origin',(-63.9999999999999,-41.3725830020309,2.23454805685961E-13));
#6236=CARTESIAN_POINT('',(-71.9999999999999,-41.3725830020309,2.22475088246643E-13));
#6237=CARTESIAN_POINT('Origin',(70.,54.3948362858346,0.));
#6238=CARTESIAN_POINT('',(70.,57.9999999999999,6.00000000000001));
#6239=CARTESIAN_POINT('',(70.,54.3948362858346,6.00000000000001));
#6240=CARTESIAN_POINT('',(70.,57.9999999999999,-6.00000000000002));
#6241=CARTESIAN_POINT('Origin',(70.,57.9999999999999,0.));
#6242=CARTESIAN_POINT('Origin',(70.,57.9999999999999,0.));
#6243=CARTESIAN_POINT('Origin',(70.,655.255455313392,0.));
#6244=CARTESIAN_POINT('',(70.,54.3948362858346,0.));
#6245=CARTESIAN_POINT('',(69.9999999999999,655.255455313392,-1000.));
#6246=CARTESIAN_POINT('Origin',(-4.30991526433058E-13,54.3948362858343,
-70.0000000000002));
#6247=CARTESIAN_POINT('',(5.99999999999958,54.3948362858344,-70.0000000000002));
#6248=CARTESIAN_POINT('Origin',(-70.0000000000004,54.3948362858341,0.));
#6249=CARTESIAN_POINT('',(-70.0000000000004,54.3948362858341,-6.00000000000001));
#6250=CARTESIAN_POINT('Origin',(5.46623248443022E-13,54.3948362858343,70.0000000000002));
#6251=CARTESIAN_POINT('',(-5.99999999999947,54.3948362858343,70.0000000000002));
#6252=CARTESIAN_POINT('Origin',(59.4642749892765,-661.73832129271,-8.));
#6253=CARTESIAN_POINT('Origin',(59.4642749892765,-661.73832129271,8.));
#6254=CARTESIAN_POINT('Origin',(-2.70989670911976E-13,78.9999999999998,
0.));
#6255=CARTESIAN_POINT('Origin',(-2.7601072278848E-13,78.9999999999998,-40.999999999998));
#6256=CARTESIAN_POINT('Origin',(2.22966184927575E-13,-65.0000000000003,
0.));
#6257=CARTESIAN_POINT('Origin',(2.12801616494652E-13,-65.0000000000003,
-82.9999999999998));
#6258=CARTESIAN_POINT('',(0.,0.,0.));
#6259=CARTESIAN_POINT('Origin',(26.,0.,0.));
#6260=CARTESIAN_POINT('',(-25.9229627936314,0.,-2.));
#6261=CARTESIAN_POINT('',(-1.99999999999991,0.,-25.9229627936314));
#6262=CARTESIAN_POINT('Origin',(0.,0.,0.));
#6263=CARTESIAN_POINT('',(-2.,0.,-2.));
#6264=CARTESIAN_POINT('',(-1.99999999999999,0.,-2.));
#6265=CARTESIAN_POINT('',(-25.9229627936314,0.,-2.));
#6266=CARTESIAN_POINT('Origin',(26.,0.,0.));
#6267=CARTESIAN_POINT('',(2.00000000000001,0.,-2.));
#6268=CARTESIAN_POINT('',(25.9229627936314,0.,-2.));
#6269=CARTESIAN_POINT('',(2.00000000000001,0.,-2.));
#6270=CARTESIAN_POINT('',(2.00000000000009,0.,-25.9229627936314));
#6271=CARTESIAN_POINT('',(2.00000000000009,0.,-25.9229627936314));
#6272=CARTESIAN_POINT('Origin',(0.,0.,0.));
#6273=CARTESIAN_POINT('Origin',(26.,0.,0.));
#6274=CARTESIAN_POINT('',(-2.00000000000001,0.,2.));
#6275=CARTESIAN_POINT('',(-25.9229627936314,0.,2.));
#6276=CARTESIAN_POINT('',(-2.00000000000001,0.,2.));
#6277=CARTESIAN_POINT('',(-2.00000000000009,0.,25.9229627936314));
#6278=CARTESIAN_POINT('',(-2.00000000000009,0.,25.9229627936314));
#6279=CARTESIAN_POINT('Origin',(0.,0.,0.));
#6280=CARTESIAN_POINT('Origin',(26.,0.,0.));
#6281=CARTESIAN_POINT('',(25.9229627936314,0.,2.));
#6282=CARTESIAN_POINT('',(1.99999999999991,0.,25.9229627936315));
#6283=CARTESIAN_POINT('Origin',(0.,0.,0.));
#6284=CARTESIAN_POINT('',(2.,0.,2.));
#6285=CARTESIAN_POINT('',(1.99999999999999,0.,2.));
#6286=CARTESIAN_POINT('',(25.9229627936314,0.,2.));
#6287=CARTESIAN_POINT('Origin',(-25.9229627936314,-24.,2.));
#6288=CARTESIAN_POINT('',(-25.9229627936314,-20.,2.));
#6289=CARTESIAN_POINT('',(-25.9229627936314,-20.,2.));
#6290=CARTESIAN_POINT('',(-21.9089023002066,-24.,2.));
#6291=CARTESIAN_POINT('Ctrl Pts',(-25.9229627936293,-20.0000000000019,2.));
#6292=CARTESIAN_POINT('Ctrl Pts',(-23.7486800263697,-22.1678404337906,2.));
#6293=CARTESIAN_POINT('Ctrl Pts',(-21.9089023002066,-24.,2.));
#6294=CARTESIAN_POINT('',(-2.,-24.,2.));
#6295=CARTESIAN_POINT('',(-2.,-24.,2.));
#6296=CARTESIAN_POINT('',(-2.00000000000002,0.,2.));
#6297=CARTESIAN_POINT('Origin',(-25.9229627936314,-24.,2.));
#6298=CARTESIAN_POINT('',(21.9089023002066,-24.,2.));
#6299=CARTESIAN_POINT('',(1.99999999999999,-24.,2.));
#6300=CARTESIAN_POINT('',(21.9089023002066,-24.,2.));
#6301=CARTESIAN_POINT('',(25.9229627936314,-20.,2.));
#6302=CARTESIAN_POINT('Ctrl Pts',(21.9089023002321,-23.9999999999746,2.));
#6303=CARTESIAN_POINT('Ctrl Pts',(23.7486800263847,-22.1678404337756,2.));
#6304=CARTESIAN_POINT('Ctrl Pts',(25.9229627936293,-20.0000000000019,2.));
#6305=CARTESIAN_POINT('',(25.9229627936314,-20.,2.));
#6306=CARTESIAN_POINT('',(1.99999999999998,-24.,2.));
#6307=CARTESIAN_POINT('Origin',(-25.9229627936314,-24.,-2.));
#6308=CARTESIAN_POINT('',(-21.9089023002066,-24.,-2.));
#6309=CARTESIAN_POINT('',(-1.99999999999999,-24.,-2.));
#6310=CARTESIAN_POINT('',(-21.9089023002066,-24.,-2.));
#6311=CARTESIAN_POINT('',(-25.9229627936314,-20.,-2.));
#6312=CARTESIAN_POINT('Ctrl Pts',(-21.9089023002321,-23.9999999999746,-2.));
#6313=CARTESIAN_POINT('Ctrl Pts',(-23.7486800263847,-22.1678404337756,-2.));
#6314=CARTESIAN_POINT('Ctrl Pts',(-25.9229627936293,-20.0000000000019,-2.));
#6315=CARTESIAN_POINT('',(-25.9229627936314,-20.,-2.));
#6316=CARTESIAN_POINT('',(-1.99999999999998,-24.,-2.));
#6317=CARTESIAN_POINT('Origin',(-25.9229627936314,-24.,-2.));
#6318=CARTESIAN_POINT('',(25.9229627936314,-20.,-2.));
#6319=CARTESIAN_POINT('',(25.9229627936314,-20.,-2.));
#6320=CARTESIAN_POINT('',(21.9089023002066,-24.,-2.));
#6321=CARTESIAN_POINT('Ctrl Pts',(25.9229627936293,-20.0000000000019,-2.));
#6322=CARTESIAN_POINT('Ctrl Pts',(23.7486800263697,-22.1678404337906,-2.));
#6323=CARTESIAN_POINT('Ctrl Pts',(21.9089023002066,-24.,-2.));
#6324=CARTESIAN_POINT('',(2.,-24.,-2.));
#6325=CARTESIAN_POINT('',(2.,-24.,-2.));
#6326=CARTESIAN_POINT('',(2.00000000000002,0.,-2.));
#6327=CARTESIAN_POINT('Origin',(0.,30.,0.));
#6328=CARTESIAN_POINT('',(-2.93915231795365E-15,30.,24.));
#6329=CARTESIAN_POINT('Origin',(0.,30.,0.));
#6330=CARTESIAN_POINT('',(0.,30.,11.));
#6331=CARTESIAN_POINT('Origin',(0.,30.,0.));
#6332=CARTESIAN_POINT('Origin',(0.,0.,0.));
#6333=CARTESIAN_POINT('',(-16.,24.,17.8885438199983));
#6334=CARTESIAN_POINT('',(-16.,8.,17.8885438199983));
#6335=CARTESIAN_POINT('',(-16.,24.,17.8885438199983));
#6336=CARTESIAN_POINT('',(-2.93915231795365E-15,24.,24.));
#6337=CARTESIAN_POINT('Origin',(0.,24.,0.));
#6338=CARTESIAN_POINT('',(-2.93915231795365E-15,0.,24.));
#6339=CARTESIAN_POINT('',(16.,24.,17.8885438199983));
#6340=CARTESIAN_POINT('Origin',(0.,24.,0.));
#6341=CARTESIAN_POINT('',(16.,8.,17.8885438199983));
#6342=CARTESIAN_POINT('',(16.,24.,17.8885438199983));
#6343=CARTESIAN_POINT('',(16.,8.,-17.8885438199983));
#6344=CARTESIAN_POINT('Origin',(0.,8.,0.));
#6345=CARTESIAN_POINT('',(16.,24.,-17.8885438199983));
#6346=CARTESIAN_POINT('',(16.,24.,-17.8885438199983));
#6347=CARTESIAN_POINT('',(-16.,24.,-17.8885438199983));
#6348=CARTESIAN_POINT('Origin',(0.,24.,0.));
#6349=CARTESIAN_POINT('',(-16.,8.,-17.8885438199983));
#6350=CARTESIAN_POINT('',(-16.,24.,-17.8885438199983));
#6351=CARTESIAN_POINT('Origin',(0.,8.,0.));
#6352=CARTESIAN_POINT('Origin',(24.,8.,0.));
#6353=CARTESIAN_POINT('',(-3.67394039744206E-15,8.,30.));
#6354=CARTESIAN_POINT('Origin',(0.,8.,0.));
#6355=CARTESIAN_POINT('',(16.,8.,-17.8885438199983));
#6356=CARTESIAN_POINT('',(-16.,8.,-17.8885438199983));
#6357=CARTESIAN_POINT('Origin',(0.,0.,0.));
#6358=CARTESIAN_POINT('',(0.,4.,-30.));
#6359=CARTESIAN_POINT('',(-3.67394039744206E-15,4.,30.));
#6360=CARTESIAN_POINT('Origin',(0.,4.,0.));
#6361=CARTESIAN_POINT('Origin',(0.,4.,0.));
#6362=CARTESIAN_POINT('',(-3.67394039744206E-15,0.,30.));
#6363=CARTESIAN_POINT('Origin',(0.,0.,0.));
#6364=CARTESIAN_POINT('',(-3.18408167778312E-15,-2.35143570712168E-15,-26.));
#6365=CARTESIAN_POINT('',(-3.18408167778312E-15,0.,-26.));
#6366=CARTESIAN_POINT('Origin',(0.,0.,0.));
#6367=CARTESIAN_POINT('Origin',(0.,0.,0.));
#6368=CARTESIAN_POINT('Origin',(0.,0.,0.));
#6369=CARTESIAN_POINT('Origin',(0.,0.,0.));
#6370=CARTESIAN_POINT('Origin',(0.,0.,0.));
#6371=CARTESIAN_POINT('Origin',(-16.,8.,-30.));
#6372=CARTESIAN_POINT('',(-16.,24.,-17.8885438199983));
#6373=CARTESIAN_POINT('Origin',(-16.,24.,-30.));
#6374=CARTESIAN_POINT('',(16.,24.,-17.8885438199983));
#6375=CARTESIAN_POINT('',(0.,24.,11.));
#6376=CARTESIAN_POINT('Origin',(0.,24.,0.));
#6377=CARTESIAN_POINT('Origin',(16.,8.,-30.));
#6378=CARTESIAN_POINT('Origin',(0.,30.000012,0.));
#6379=CARTESIAN_POINT('',(-1.34711147906209E-15,30.000012,11.));
#6380=CARTESIAN_POINT('Origin',(0.,-24.,0.));
#6381=CARTESIAN_POINT('Origin',(0.,-20.,0.));
#6382=CARTESIAN_POINT('Origin',(0.,-24.,0.));
#6383=CARTESIAN_POINT('Origin',(0.,-20.,0.));
#6384=CARTESIAN_POINT('Origin',(0.,-24.,0.));
#6385=CARTESIAN_POINT('',(1.99999999999992,-24.,21.9089023002066));
#6386=CARTESIAN_POINT('',(1.99999999999999,-24.,2.));
#6387=CARTESIAN_POINT('',(-2.00000000000008,-24.,21.9089023002066));
#6388=CARTESIAN_POINT('Origin',(0.,-24.,0.));
#6389=CARTESIAN_POINT('',(-2.00000000000008,-24.,21.9089023002066));
#6390=CARTESIAN_POINT('Origin',(0.,-24.,0.));
#6391=CARTESIAN_POINT('',(-1.99999999999992,-24.,-21.9089023002066));
#6392=CARTESIAN_POINT('',(-1.99999999999999,-24.,-2.));
#6393=CARTESIAN_POINT('',(2.00000000000008,-24.,-21.9089023002066));
#6394=CARTESIAN_POINT('Origin',(0.,-24.,0.));
#6395=CARTESIAN_POINT('',(2.00000000000008,-24.,-21.9089023002066));
#6396=CARTESIAN_POINT('Origin',(0.,-24.,0.));
#6397=CARTESIAN_POINT('Origin',(2.00000000000009,-24.,-25.9229627936314));
#6398=CARTESIAN_POINT('',(2.00000000000009,-20.,-25.9229627936314));
#6399=CARTESIAN_POINT('Ctrl Pts',(2.00000000000008,-23.9999999999746,-21.9089023002321));
#6400=CARTESIAN_POINT('Ctrl Pts',(2.00000000000008,-22.1678404337738,-23.7486800263865));
#6401=CARTESIAN_POINT('Ctrl Pts',(2.00000000000009,-20.0000000000019,-25.9229627936293));
#6402=CARTESIAN_POINT('',(2.00000000000009,-20.,-25.9229627936314));
#6403=CARTESIAN_POINT('Origin',(-1.99999999999991,-24.,-25.9229627936314));
#6404=CARTESIAN_POINT('',(-1.99999999999991,-20.,-25.9229627936314));
#6405=CARTESIAN_POINT('',(-1.99999999999991,-20.,-25.9229627936314));
#6406=CARTESIAN_POINT('Ctrl Pts',(-1.99999999999991,-20.0000000000021,-25.9229627936295));
#6407=CARTESIAN_POINT('Ctrl Pts',(-1.99999999999992,-22.167840433814,-23.7486800263466));
#6408=CARTESIAN_POINT('Ctrl Pts',(-1.99999999999992,-24.,-21.9089023002067));
#6409=CARTESIAN_POINT('Origin',(0.,-24.,0.));
#6410=CARTESIAN_POINT('Origin',(0.,-20.,0.));
#6411=CARTESIAN_POINT('Origin',(-1.99999999999991,-24.,-25.9229627936314));
#6412=CARTESIAN_POINT('',(-2.00000000000009,-20.,25.9229627936314));
#6413=CARTESIAN_POINT('Ctrl Pts',(-2.00000000000008,-23.9999999999746,21.9089023002321));
#6414=CARTESIAN_POINT('Ctrl Pts',(-2.00000000000008,-22.1678404337738,23.7486800263865));
#6415=CARTESIAN_POINT('Ctrl Pts',(-2.00000000000009,-20.0000000000019,25.9229627936293));
#6416=CARTESIAN_POINT('',(-2.00000000000009,-20.,25.9229627936314));
#6417=CARTESIAN_POINT('Origin',(2.00000000000009,-24.,-25.9229627936314));
#6418=CARTESIAN_POINT('',(1.99999999999991,-20.,25.9229627936315));
#6419=CARTESIAN_POINT('',(1.99999999999991,-20.,25.9229627936315));
#6420=CARTESIAN_POINT('Ctrl Pts',(1.99999999999991,-20.0000000000021,25.9229627936295));
#6421=CARTESIAN_POINT('Ctrl Pts',(1.99999999999992,-22.1678404338147,23.7486800263459));
#6422=CARTESIAN_POINT('Ctrl Pts',(1.99999999999992,-24.,21.9089023002067));
#6423=CARTESIAN_POINT('Origin',(0.,-24.,0.));
#6424=CARTESIAN_POINT('Origin',(0.,-20.,0.));
#6425=CARTESIAN_POINT('Origin',(0.,-24.,0.));
#6426=CARTESIAN_POINT('Origin',(0.,-24.,0.));
#6427=CARTESIAN_POINT('Origin',(0.,-24.,0.));
#6428=CARTESIAN_POINT('Origin',(0.,-24.,0.));
#6429=CARTESIAN_POINT('',(0.,0.,0.));
#6430=CARTESIAN_POINT('Origin',(232.,0.,0.));
#6431=CARTESIAN_POINT('',(232.,8.67361737988404E-16,-6.));
#6432=CARTESIAN_POINT('',(232.,6.,0.));
#6433=CARTESIAN_POINT('Origin',(232.,0.,0.));
#6434=CARTESIAN_POINT('',(232.,6.,-6.));
#6435=CARTESIAN_POINT('',(232.,8.67361737988404E-16,-6.));
#6436=CARTESIAN_POINT('',(232.,6.,-6.));
#6437=CARTESIAN_POINT('Origin',(232.,0.,0.));
#6438=CARTESIAN_POINT('',(232.,-8.67361737988403E-16,6.));
#6439=CARTESIAN_POINT('Origin',(232.,0.,0.));
#6440=CARTESIAN_POINT('',(232.,6.,6.));
#6441=CARTESIAN_POINT('',(232.,6.,0.));
#6442=CARTESIAN_POINT('',(232.,6.,6.));
#6443=CARTESIAN_POINT('Origin',(232.,0.,0.));
#6444=CARTESIAN_POINT('',(232.,-6.,-8.67361737988403E-16));
#6445=CARTESIAN_POINT('Origin',(232.,0.,0.));
#6446=CARTESIAN_POINT('',(232.,-6.,6.));
#6447=CARTESIAN_POINT('',(232.,8.67361737988404E-16,6.));
#6448=CARTESIAN_POINT('',(232.,-6.,6.));
#6449=CARTESIAN_POINT('Origin',(0.,-8.,0.));
#6450=CARTESIAN_POINT('',(0.,-8.57252759403147E-16,-7.));
#6451=CARTESIAN_POINT('Origin',(0.,0.,0.));
#6452=CARTESIAN_POINT('Origin',(216.,0.,0.));
#6453=CARTESIAN_POINT('',(216.,-1.22464679914735E-15,-9.99999999999998));
#6454=CARTESIAN_POINT('Origin',(216.,0.,0.));
#6455=CARTESIAN_POINT('',(216.,-6.,-6.));
#6456=CARTESIAN_POINT('',(216.,6.,-6.));
#6457=CARTESIAN_POINT('',(216.,-6.,-6.));
#6458=CARTESIAN_POINT('',(216.,-6.,6.));
#6459=CARTESIAN_POINT('',(216.,-6.,6.));
#6460=CARTESIAN_POINT('',(216.,6.,6.));
#6461=CARTESIAN_POINT('',(216.,6.,6.));
#6462=CARTESIAN_POINT('',(216.,6.,-6.));
#6463=CARTESIAN_POINT('Origin',(0.,0.,0.));
#6464=CARTESIAN_POINT('',(22.,-1.22464679914735E-15,-9.99999999999998));
#6465=CARTESIAN_POINT('Origin',(22.,0.,0.));
#6466=CARTESIAN_POINT('',(0.,-1.22464679914735E-15,-9.99999999999998));
#6467=CARTESIAN_POINT('Origin',(22.,-10.,0.));
#6468=CARTESIAN_POINT('',(22.,-9.79717439317882E-16,-8.));
#6469=CARTESIAN_POINT('Origin',(22.,0.,0.));
#6470=CARTESIAN_POINT('Origin',(0.,0.,0.));
#6471=CARTESIAN_POINT('',(1.,-9.79717439317882E-16,-8.));
#6472=CARTESIAN_POINT('Origin',(1.,0.,0.));
#6473=CARTESIAN_POINT('',(0.,-9.79717439317882E-16,-8.));
#6474=CARTESIAN_POINT('',(10.,-7.74596669241483,2.));
#6475=CARTESIAN_POINT('',(10.,-7.74596669241483,-2.));
#6476=CARTESIAN_POINT('Ctrl Pts',(10.,-7.74596669241483,2.));
#6477=CARTESIAN_POINT('Ctrl Pts',(9.74770117864322,-7.74596669241483,2.));
#6478=CARTESIAN_POINT('Ctrl Pts',(9.479356583979,-7.75957726931369,1.94935810817991));
#6479=CARTESIAN_POINT('Ctrl Pts',(8.98693862993913,-7.8080895555786,1.74492797023227));
#6480=CARTESIAN_POINT('Ctrl Pts',(8.76276709090545,-7.84222121032682,1.59119421565164));
#6481=CARTESIAN_POINT('Ctrl Pts',(8.40883052939687,-7.90579009335489,1.23725765414306));
#6482=CARTESIAN_POINT('Ctrl Pts',(8.25507748138546,-7.93945007560673,1.01307580920409));
#6483=CARTESIAN_POINT('Ctrl Pts',(8.05063325793989,-7.98687320195912,0.520621311632992));
#6484=CARTESIAN_POINT('Ctrl Pts',(8.,-8.,0.252263545486474));
#6485=CARTESIAN_POINT('Ctrl Pts',(8.,-8.,-0.252263545486473));
#6486=CARTESIAN_POINT('Ctrl Pts',(8.05063325793989,-7.98687320195912,-0.52062131163299));
#6487=CARTESIAN_POINT('Ctrl Pts',(8.25507748138546,-7.93945007560673,-1.01307580920409));
#6488=CARTESIAN_POINT('Ctrl Pts',(8.40883052939687,-7.90579009335489,-1.23725765414306));
#6489=CARTESIAN_POINT('Ctrl Pts',(8.76276709090545,-7.84222121032682,-1.59119421565164));
#6490=CARTESIAN_POINT('Ctrl Pts',(8.98693862993913,-7.8080895555786,-1.74492797023227));
#6491=CARTESIAN_POINT('Ctrl Pts',(9.479356583979,-7.75957726931369,-1.94935810817991));
#6492=CARTESIAN_POINT('Ctrl Pts',(9.74770117864322,-7.74596669241483,-2.));
#6493=CARTESIAN_POINT('Ctrl Pts',(10.,-7.74596669241483,-2.));
#6494=CARTESIAN_POINT('Ctrl Pts',(10.,-7.74596669241483,-2.));
#6495=CARTESIAN_POINT('Ctrl Pts',(10.2522988213568,-7.74596669241483,-2.));
#6496=CARTESIAN_POINT('Ctrl Pts',(10.520643416021,-7.75957726931369,-1.94935810817991));
#6497=CARTESIAN_POINT('Ctrl Pts',(11.0130613700609,-7.8080895555786,-1.74492797023227));
#6498=CARTESIAN_POINT('Ctrl Pts',(11.2372329090946,-7.84222121032682,-1.59119421565164));
#6499=CARTESIAN_POINT('Ctrl Pts',(11.5911694706031,-7.90579009335489,-1.23725765414306));
#6500=CARTESIAN_POINT('Ctrl Pts',(11.7449225186145,-7.93945007560673,-1.01307580920409));
#6501=CARTESIAN_POINT('Ctrl Pts',(11.9493667420601,-7.98687320195912,-0.520621311632991));
#6502=CARTESIAN_POINT('Ctrl Pts',(12.,-8.,-0.252263545486473));
#6503=CARTESIAN_POINT('Ctrl Pts',(12.,-8.,0.252263545486474));
#6504=CARTESIAN_POINT('Ctrl Pts',(11.9493667420601,-7.98687320195912,0.520621311632992));
#6505=CARTESIAN_POINT('Ctrl Pts',(11.7449225186145,-7.93945007560673,1.01307580920409));
#6506=CARTESIAN_POINT('Ctrl Pts',(11.5911694706031,-7.90579009335489,1.23725765414306));
#6507=CARTESIAN_POINT('Ctrl Pts',(11.2372329090946,-7.84222121032682,1.59119421565164));
#6508=CARTESIAN_POINT('Ctrl Pts',(11.0130613700609,-7.8080895555786,1.74492797023227));
#6509=CARTESIAN_POINT('Ctrl Pts',(10.520643416021,-7.75957726931369,1.94935810817991));
#6510=CARTESIAN_POINT('Ctrl Pts',(10.2522988213568,-7.74596669241483,2.));
#6511=CARTESIAN_POINT('Ctrl Pts',(10.,-7.74596669241483,2.));
#6512=CARTESIAN_POINT('',(10.,7.74596669241483,2.));
#6513=CARTESIAN_POINT('',(10.,7.74596669241483,-2.));
#6514=CARTESIAN_POINT('Ctrl Pts',(10.,7.74596669241483,2.));
#6515=CARTESIAN_POINT('Ctrl Pts',(10.2522988213568,7.74596669241483,2.));
#6516=CARTESIAN_POINT('Ctrl Pts',(10.520643416021,7.75957726931369,1.94935810817991));
#6517=CARTESIAN_POINT('Ctrl Pts',(11.0130613700609,7.8080895555786,1.74492797023227));
#6518=CARTESIAN_POINT('Ctrl Pts',(11.2372329090946,7.84222121032682,1.59119421565164));
#6519=CARTESIAN_POINT('Ctrl Pts',(11.5911694706031,7.90579009335489,1.23725765414306));
#6520=CARTESIAN_POINT('Ctrl Pts',(11.7449225186145,7.93945007560673,1.01307580920409));
#6521=CARTESIAN_POINT('Ctrl Pts',(11.9493667420601,7.98687320195912,0.520621311632992));
#6522=CARTESIAN_POINT('Ctrl Pts',(12.,8.,0.252263545486474));
#6523=CARTESIAN_POINT('Ctrl Pts',(12.,8.,-0.252263545486473));
#6524=CARTESIAN_POINT('Ctrl Pts',(11.9493667420601,7.98687320195912,-0.520621311632991));
#6525=CARTESIAN_POINT('Ctrl Pts',(11.7449225186145,7.93945007560673,-1.01307580920409));
#6526=CARTESIAN_POINT('Ctrl Pts',(11.5911694706031,7.90579009335489,-1.23725765414306));
#6527=CARTESIAN_POINT('Ctrl Pts',(11.2372329090946,7.84222121032682,-1.59119421565164));
#6528=CARTESIAN_POINT('Ctrl Pts',(11.0130613700609,7.8080895555786,-1.74492797023227));
#6529=CARTESIAN_POINT('Ctrl Pts',(10.520643416021,7.75957726931369,-1.94935810817991));
#6530=CARTESIAN_POINT('Ctrl Pts',(10.2522988213568,7.74596669241483,-2.));
#6531=CARTESIAN_POINT('Ctrl Pts',(10.,7.74596669241483,-2.));
#6532=CARTESIAN_POINT('Ctrl Pts',(10.,7.74596669241483,-2.));
#6533=CARTESIAN_POINT('Ctrl Pts',(9.74770117864322,7.74596669241483,-2.));
#6534=CARTESIAN_POINT('Ctrl Pts',(9.479356583979,7.75957726931369,-1.94935810817991));
#6535=CARTESIAN_POINT('Ctrl Pts',(8.98693862993913,7.8080895555786,-1.74492797023227));
#6536=CARTESIAN_POINT('Ctrl Pts',(8.76276709090545,7.84222121032682,-1.59119421565164));
#6537=CARTESIAN_POINT('Ctrl Pts',(8.40883052939687,7.90579009335489,-1.23725765414306));
#6538=CARTESIAN_POINT('Ctrl Pts',(8.25507748138546,7.93945007560673,-1.01307580920409));
#6539=CARTESIAN_POINT('Ctrl Pts',(8.05063325793989,7.98687320195912,-0.52062131163299));
#6540=CARTESIAN_POINT('Ctrl Pts',(8.,8.,-0.252263545486473));
#6541=CARTESIAN_POINT('Ctrl Pts',(8.,8.,0.252263545486474));
#6542=CARTESIAN_POINT('Ctrl Pts',(8.05063325793989,7.98687320195912,0.520621311632991));
#6543=CARTESIAN_POINT('Ctrl Pts',(8.25507748138546,7.93945007560673,1.01307580920409));
#6544=CARTESIAN_POINT('Ctrl Pts',(8.40883052939687,7.90579009335489,1.23725765414306));
#6545=CARTESIAN_POINT('Ctrl Pts',(8.76276709090545,7.84222121032682,1.59119421565164));
#6546=CARTESIAN_POINT('Ctrl Pts',(8.98693862993913,7.8080895555786,1.74492797023227));
#6547=CARTESIAN_POINT('Ctrl Pts',(9.479356583979,7.75957726931369,1.94935810817991));
#6548=CARTESIAN_POINT('Ctrl Pts',(9.74770117864322,7.74596669241483,2.));
#6549=CARTESIAN_POINT('Ctrl Pts',(10.,7.74596669241483,2.));
#6550=CARTESIAN_POINT('Origin',(10.,-10.,0.));
#6551=CARTESIAN_POINT('',(10.,-10.,-2.));
#6552=CARTESIAN_POINT('Origin',(1.,0.,0.));
#6553=CARTESIAN_POINT('Origin',(1.,-8.57252759403147E-16,-7.));
#6554=CARTESIAN_POINT('Origin',(232.,6.,-6.));
#6555=CARTESIAN_POINT('',(232.,6.,-6.));
#6556=CARTESIAN_POINT('',(232.,-6.,-6.));
#6557=CARTESIAN_POINT('',(232.,-6.,-6.));
#6558=CARTESIAN_POINT('',(232.,-6.,-6.));
#6559=CARTESIAN_POINT('Origin',(232.,6.,6.));
#6560=CARTESIAN_POINT('',(232.,6.,6.));
#6561=CARTESIAN_POINT('Origin',(232.,6.,6.));
#6562=CARTESIAN_POINT('',(232.,-6.,6.));
#6563=CARTESIAN_POINT('Origin',(232.,-6.,6.));
#6564=CARTESIAN_POINT('',(232.,-6.,-8.67361737988404E-16));
#6565=CARTESIAN_POINT('Origin',(232.,0.,0.));
#6566=CARTESIAN_POINT('Origin',(232.,0.,0.));
#6567=CARTESIAN_POINT('Origin',(256.,0.,0.));
#6568=CARTESIAN_POINT('',(256.,0.,-6.));
#6569=CARTESIAN_POINT('',(256.,-7.34788079488412E-16,-6.));
#6570=CARTESIAN_POINT('Origin',(256.,0.,0.));
#6571=CARTESIAN_POINT('Origin',(256.,0.,0.));
#6572=CARTESIAN_POINT('',(0.,0.,0.));
#6573=CARTESIAN_POINT('Origin',(0.,12.,0.));
#6574=CARTESIAN_POINT('',(0.,12.,14.));
#6575=CARTESIAN_POINT('Origin',(0.,12.,0.));
#6576=CARTESIAN_POINT('',(0.,12.,8.));
#6577=CARTESIAN_POINT('Origin',(0.,12.,0.));
#6578=CARTESIAN_POINT('Origin',(0.,0.,0.));
#6579=CARTESIAN_POINT('',(0.,0.,14.));
#6580=CARTESIAN_POINT('Origin',(0.,0.,0.));
#6581=CARTESIAN_POINT('',(0.,0.,8.));
#6582=CARTESIAN_POINT('Origin',(0.,0.,0.));
#6583=CARTESIAN_POINT('Origin',(0.,12.,0.));
#6584=CARTESIAN_POINT('',(-8.22558289883611E-16,4.,14.));
#6585=CARTESIAN_POINT('',(-1.71450551880629E-15,12.,14.));
#6586=CARTESIAN_POINT('',(-1.45802973181661,4.63299112089927,13.9238697674583));
#6587=CARTESIAN_POINT('Ctrl Pts',(6.93889390390723E-17,4.,14.));
#6588=CARTESIAN_POINT('Ctrl Pts',(-0.25151516454739,4.,14.));
#6589=CARTESIAN_POINT('Ctrl Pts',(-0.519513937917108,4.050469286675,13.9925306456456));
#6590=CARTESIAN_POINT('Ctrl Pts',(-1.01196367232324,4.25513100778376,13.9655554177696));
#6591=CARTESIAN_POINT('Ctrl Pts',(-1.23644395127912,4.40930284567681,13.9464298471224));
#6592=CARTESIAN_POINT('Ctrl Pts',(-1.42855606179944,4.60197987136062,13.9269326944353));
#6593=CARTESIAN_POINT('Ctrl Pts',(-1.44338181871977,4.61732784601981,13.9254036149562));
#6594=CARTESIAN_POINT('Ctrl Pts',(-1.45802973181661,4.63299112089927,13.9238697674583));
#6595=CARTESIAN_POINT('',(-1.99744241740809,6.,13.8567753748532));
#6596=CARTESIAN_POINT('Ctrl Pts',(-1.45802973181661,4.63299112089927,13.9238697674583));
#6597=CARTESIAN_POINT('Ctrl Pts',(-1.61634141723231,4.80227663132682,13.9072922535857));
#6598=CARTESIAN_POINT('Ctrl Pts',(-1.75242809682337,5.00975783196893,13.8902060158894));
#6599=CARTESIAN_POINT('Ctrl Pts',(-1.94731439399108,5.48114930972434,13.8642887746891));
#6600=CARTESIAN_POINT('Ctrl Pts',(-1.99744241740809,5.74885047030811,13.8567753748532));
#6601=CARTESIAN_POINT('Ctrl Pts',(-1.99744241740809,6.,13.8567753748532));
#6602=CARTESIAN_POINT('',(-7.87863820364075E-16,8.,14.));
#6603=CARTESIAN_POINT('Ctrl Pts',(-1.99744241740809,6.,13.8567753748532));
#6604=CARTESIAN_POINT('Ctrl Pts',(-1.99744241740809,6.25114952969189,13.8567753748532));
#6605=CARTESIAN_POINT('Ctrl Pts',(-1.94731439399108,6.51885069027566,13.8642887746891));
#6606=CARTESIAN_POINT('Ctrl Pts',(-1.74381075604205,7.01108581411736,13.8913520056423));
#6607=CARTESIAN_POINT('Ctrl Pts',(-1.59045163862178,7.23564848986549,13.9105021697166));
#6608=CARTESIAN_POINT('Ctrl Pts',(-1.23644395127912,7.59069715432319,13.9464298471224));
#6609=CARTESIAN_POINT('Ctrl Pts',(-1.01196367232324,7.74486899221624,13.9655554177696));
#6610=CARTESIAN_POINT('Ctrl Pts',(-0.519513937917107,7.949530713325,13.9925306456456));
#6611=CARTESIAN_POINT('Ctrl Pts',(-0.25151516454739,8.,14.));
#6612=CARTESIAN_POINT('Ctrl Pts',(1.38777878078145E-16,8.,14.));
#6613=CARTESIAN_POINT('',(-1.71450551880629E-15,12.,14.));
#6614=CARTESIAN_POINT('Ctrl Pts',(2.08166817117217E-16,8.,14.));
#6615=CARTESIAN_POINT('Ctrl Pts',(0.251515164547391,8.,14.));
#6616=CARTESIAN_POINT('Ctrl Pts',(0.519513937917107,7.949530713325,13.9925306456456));
#6617=CARTESIAN_POINT('Ctrl Pts',(1.01196367232324,7.74486899221624,13.9655554177696));
#6618=CARTESIAN_POINT('Ctrl Pts',(1.23644395127912,7.59069715432319,13.9464298471224));
#6619=CARTESIAN_POINT('Ctrl Pts',(1.59045163862178,7.23564848986549,13.9105021697166));
#6620=CARTESIAN_POINT('Ctrl Pts',(1.74381075604205,7.01108581411736,13.8913520056423));
#6621=CARTESIAN_POINT('Ctrl Pts',(1.94731439399108,6.51885069027566,13.8642887746891));
#6622=CARTESIAN_POINT('Ctrl Pts',(1.99744241740809,6.25114952969188,13.8567753748532));
#6623=CARTESIAN_POINT('Ctrl Pts',(1.99744241740809,5.74885047030811,13.8567753748532));
#6624=CARTESIAN_POINT('Ctrl Pts',(1.94731439399108,5.48114930972434,13.8642887746891));
#6625=CARTESIAN_POINT('Ctrl Pts',(1.74381075604205,4.98891418588264,13.8913520056423));
#6626=CARTESIAN_POINT('Ctrl Pts',(1.59045163862178,4.76435151013451,13.9105021697166));
#6627=CARTESIAN_POINT('Ctrl Pts',(1.23644395127912,4.40930284567681,13.9464298471224));
#6628=CARTESIAN_POINT('Ctrl Pts',(1.01196367232324,4.25513100778376,13.9655554177696));
#6629=CARTESIAN_POINT('Ctrl Pts',(0.519513937917108,4.050469286675,13.9925306456456));
#6630=CARTESIAN_POINT('Ctrl Pts',(0.251515164547391,4.,14.));
#6631=CARTESIAN_POINT('Ctrl Pts',(2.08166817117217E-16,4.,14.));
#6632=CARTESIAN_POINT('',(-1.08344435620045,4.96154049110382,-13.9580137672599));
#6633=CARTESIAN_POINT('',(-1.50144186694001,6.,-13.9192554513594));
#6634=CARTESIAN_POINT('Ctrl Pts',(-1.08344435620045,4.96154049110382,-13.9580137672599));
#6635=CARTESIAN_POINT('Ctrl Pts',(-1.0761391389456,4.95393345386291,-13.9585808104322));
#6636=CARTESIAN_POINT('Ctrl Pts',(-1.06877893978868,4.94642971506651,-13.9591463493795));
#6637=CARTESIAN_POINT('Ctrl Pts',(-0.928120699239766,4.80598855727717,-13.969840718405));
#6638=CARTESIAN_POINT('Ctrl Pts',(-0.75939870112794,4.69065402980549,-13.980613498328));
#6639=CARTESIAN_POINT('Ctrl Pts',(-0.389628419705622,4.53765624525252,-13.9958004369066));
#6640=CARTESIAN_POINT('Ctrl Pts',(-0.18856845269616,4.5,-14.));
#6641=CARTESIAN_POINT('Ctrl Pts',(0.188568452696161,4.5,-14.));
#6642=CARTESIAN_POINT('Ctrl Pts',(0.389628419705623,4.53765624525252,-13.9958004369066));
#6643=CARTESIAN_POINT('Ctrl Pts',(0.75939870112794,4.69065402980549,-13.980613498328));
#6644=CARTESIAN_POINT('Ctrl Pts',(0.928120699239766,4.80598855727717,-13.969840718405));
#6645=CARTESIAN_POINT('Ctrl Pts',(1.19464720522372,5.07210372362547,-13.9495764750947));
#6646=CARTESIAN_POINT('Ctrl Pts',(1.31025681386282,5.24069144342751,-13.9387649526973));
#6647=CARTESIAN_POINT('Ctrl Pts',(1.4636586514978,5.61032763153242,-13.9234925472081));
#6648=CARTESIAN_POINT('Ctrl Pts',(1.50144186694001,5.81138905279535,-13.9192554513594));
#6649=CARTESIAN_POINT('Ctrl Pts',(1.50144186694001,6.18861094720465,-13.9192554513594));
#6650=CARTESIAN_POINT('Ctrl Pts',(1.4636586514978,6.38967236846757,-13.9234925472081));
#6651=CARTESIAN_POINT('Ctrl Pts',(1.31025681386282,6.75930855657249,-13.9387649526973));
#6652=CARTESIAN_POINT('Ctrl Pts',(1.19464720522372,6.92789627637453,-13.9495764750947));
#6653=CARTESIAN_POINT('Ctrl Pts',(0.928120699239766,7.19401144272283,-13.969840718405));
#6654=CARTESIAN_POINT('Ctrl Pts',(0.75939870112794,7.30934597019451,-13.980613498328));
#6655=CARTESIAN_POINT('Ctrl Pts',(0.389628419705623,7.46234375474748,-13.9958004369066));
#6656=CARTESIAN_POINT('Ctrl Pts',(0.188568452696161,7.5,-14.));
#6657=CARTESIAN_POINT('Ctrl Pts',(-0.188568452696161,7.5,-14.));
#6658=CARTESIAN_POINT('Ctrl Pts',(-0.389628419705623,7.46234375474748,-13.9958004369066));
#6659=CARTESIAN_POINT('Ctrl Pts',(-0.75939870112794,7.30934597019451,-13.980613498328));
#6660=CARTESIAN_POINT('Ctrl Pts',(-0.928120699239766,7.19401144272283,-13.969840718405));
#6661=CARTESIAN_POINT('Ctrl Pts',(-1.19464720522372,6.92789627637453,-13.9495764750947));
#6662=CARTESIAN_POINT('Ctrl Pts',(-1.31025681386282,6.75930855657249,-13.9387649526973));
#6663=CARTESIAN_POINT('Ctrl Pts',(-1.4636586514978,6.38967236846757,-13.9234925472081));
#6664=CARTESIAN_POINT('Ctrl Pts',(-1.50144186694001,6.18861094720465,-13.9192554513594));
#6665=CARTESIAN_POINT('Ctrl Pts',(-1.50144186694001,6.,-13.9192554513594));
#6666=CARTESIAN_POINT('Ctrl Pts',(-1.50144186694001,6.,-13.9192554513594));
#6667=CARTESIAN_POINT('Ctrl Pts',(-1.50144186694001,5.81138905279535,-13.9192554513594));
#6668=CARTESIAN_POINT('Ctrl Pts',(-1.4636586514978,5.61032763153242,-13.9234925472081));
#6669=CARTESIAN_POINT('Ctrl Pts',(-1.31452122949328,5.25096695487144,-13.9383403953016));
#6670=CARTESIAN_POINT('Ctrl Pts',(-1.20753272816477,5.09075565798599,-13.9483818204431));
#6671=CARTESIAN_POINT('Ctrl Pts',(-1.08344435620045,4.96154049110382,-13.9580137672599));
#6672=CARTESIAN_POINT('Origin',(0.,12.,0.));
#6673=CARTESIAN_POINT('',(-4.89858719658941E-16,7.89285714285714,8.));
#6674=CARTESIAN_POINT('',(-9.79717439317883E-16,12.,8.));
#6675=CARTESIAN_POINT('',(-1.8888183153337,6.,7.77382565868698));
#6676=CARTESIAN_POINT('Ctrl Pts',(-1.8888183153337,6.,7.77382565868698));
#6677=CARTESIAN_POINT('Ctrl Pts',(-1.8888183153337,6.23809453816994,7.77382565868698));
#6678=CARTESIAN_POINT('Ctrl Pts',(-1.84126818534383,6.49149873782234,7.78584860900432));
#6679=CARTESIAN_POINT('Ctrl Pts',(-1.64896551578976,6.95689762810345,7.8288325824729));
#6680=CARTESIAN_POINT('Ctrl Pts',(-1.50425576119276,7.16897165737161,7.85912333726051));
#6681=CARTESIAN_POINT('Ctrl Pts',(-1.17034427142268,7.50455135351629,7.91574638772443));
#6682=CARTESIAN_POINT('Ctrl Pts',(-0.958382508360478,7.65058083501241,7.94582869803651));
#6683=CARTESIAN_POINT('Ctrl Pts',(-0.492588734304788,7.84475933338953,7.98824430458773));
#6684=CARTESIAN_POINT('Ctrl Pts',(-0.238682962671764,7.89285714285714,8.));
#6685=CARTESIAN_POINT('Ctrl Pts',(6.93889390390723E-17,7.89285714285714,
8.));
#6686=CARTESIAN_POINT('',(-1.37403979594041,4.70119646738038,7.88111760089723));
#6687=CARTESIAN_POINT('Ctrl Pts',(-1.37403979594041,4.70119646738038,7.88111760089723));
#6688=CARTESIAN_POINT('Ctrl Pts',(-1.52556322669951,4.86218398763909,7.85470012631764));
#6689=CARTESIAN_POINT('Ctrl Pts',(-1.65605343215512,5.06025610365957,7.82724827368664));
#6690=CARTESIAN_POINT('Ctrl Pts',(-1.84126818534383,5.50850126217766,7.78584860900432));
#6691=CARTESIAN_POINT('Ctrl Pts',(-1.8888183153337,5.76190546183006,7.77382565868698));
#6692=CARTESIAN_POINT('Ctrl Pts',(-1.8888183153337,6.,7.77382565868698));
#6693=CARTESIAN_POINT('',(-7.32720006295694E-16,4.10714285714286,8.));
#6694=CARTESIAN_POINT('Ctrl Pts',(0.,4.10714285714286,8.));
#6695=CARTESIAN_POINT('Ctrl Pts',(-0.238682962671764,4.10714285714286,8.));
#6696=CARTESIAN_POINT('Ctrl Pts',(-0.492588734304787,4.15524066661047,7.98824430458773));
#6697=CARTESIAN_POINT('Ctrl Pts',(-0.958382508360477,4.34941916498759,7.94582869803651));
#6698=CARTESIAN_POINT('Ctrl Pts',(-1.17034427142268,4.49544864648371,7.91574638772443));
#6699=CARTESIAN_POINT('Ctrl Pts',(-1.34979823107329,4.67579914982511,7.88531547736479));
#6700=CARTESIAN_POINT('Ctrl Pts',(-1.3619811367988,4.68838462948094,7.88321997753786));
#6701=CARTESIAN_POINT('Ctrl Pts',(-1.37403979594041,4.70119646738038,7.88111760089723));
#6702=CARTESIAN_POINT('',(-9.79717439317883E-16,12.,8.));
#6703=CARTESIAN_POINT('Ctrl Pts',(6.93889390390723E-17,7.89285714285714,
8.));
#6704=CARTESIAN_POINT('Ctrl Pts',(0.238682962671764,7.89285714285714,8.));
#6705=CARTESIAN_POINT('Ctrl Pts',(0.492588734304788,7.84475933338953,7.98824430458773));
#6706=CARTESIAN_POINT('Ctrl Pts',(0.958382508360478,7.65058083501241,7.94582869803651));
#6707=CARTESIAN_POINT('Ctrl Pts',(1.17034427142268,7.50455135351629,7.91574638772443));
#6708=CARTESIAN_POINT('Ctrl Pts',(1.50425576119275,7.16897165737161,7.85912333726051));
#6709=CARTESIAN_POINT('Ctrl Pts',(1.64896551578976,6.95689762810345,7.8288325824729));
#6710=CARTESIAN_POINT('Ctrl Pts',(1.84126818534383,6.49149873782234,7.78584860900432));
#6711=CARTESIAN_POINT('Ctrl Pts',(1.8888183153337,6.23809453816994,7.77382565868698));
#6712=CARTESIAN_POINT('Ctrl Pts',(1.8888183153337,5.76190546183006,7.77382565868698));
#6713=CARTESIAN_POINT('Ctrl Pts',(1.84126818534383,5.50850126217766,7.78584860900432));
#6714=CARTESIAN_POINT('Ctrl Pts',(1.64896551578976,5.04310237189655,7.8288325824729));
#6715=CARTESIAN_POINT('Ctrl Pts',(1.50425576119275,4.83102834262839,7.85912333726051));
#6716=CARTESIAN_POINT('Ctrl Pts',(1.17034427142268,4.49544864648371,7.91574638772443));
#6717=CARTESIAN_POINT('Ctrl Pts',(0.958382508360478,4.34941916498759,7.94582869803651));
#6718=CARTESIAN_POINT('Ctrl Pts',(0.492588734304788,4.15524066661047,7.98824430458773));
#6719=CARTESIAN_POINT('Ctrl Pts',(0.238682962671764,4.10714285714286,8.));
#6720=CARTESIAN_POINT('Ctrl Pts',(-2.77555756156289E-16,4.10714285714286,
8.));
#6721=CARTESIAN_POINT('',(-1.17898168752143,4.90550167217474,-7.91264824066438));
#6722=CARTESIAN_POINT('',(-1.61006596901441,6.,-7.83630573519319));
#6723=CARTESIAN_POINT('Ctrl Pts',(-1.17898168752143,4.90550167217474,-7.91264824066438));
#6724=CARTESIAN_POINT('Ctrl Pts',(-1.16545353798237,4.89098220165951,-7.91466392998703));
#6725=CARTESIAN_POINT('Ctrl Pts',(-1.15173426773385,4.87679671704893,-7.91667258611177));
#6726=CARTESIAN_POINT('Ctrl Pts',(-0.995172181265423,4.72069148871753,-7.93916938835585));
#6727=CARTESIAN_POINT('Ctrl Pts',(-0.814524503839801,4.5972583768551,-7.96090747080436));
#6728=CARTESIAN_POINT('Ctrl Pts',(-0.418224335279089,4.43332696536825,-7.99153216392396));
#6729=CARTESIAN_POINT('Ctrl Pts',(-0.202527815380415,4.39285714285714,-8.));
#6730=CARTESIAN_POINT('Ctrl Pts',(0.202527815380416,4.39285714285714,-8.));
#6731=CARTESIAN_POINT('Ctrl Pts',(0.418224335279089,4.43332696536825,-7.99153216392396));
#6732=CARTESIAN_POINT('Ctrl Pts',(0.814524503839801,4.5972583768551,-7.96090747080436));
#6733=CARTESIAN_POINT('Ctrl Pts',(0.995172181265423,4.72069148871753,-7.93916938835585));
#6734=CARTESIAN_POINT('Ctrl Pts',(1.28060364728793,5.00529004754802,-7.89815501897568));
#6735=CARTESIAN_POINT('Ctrl Pts',(1.40458789962237,5.18566238393601,-7.876176798428));
#6736=CARTESIAN_POINT('Ctrl Pts',(1.5693348410951,5.58167896973006,-7.84501220025286));
#6737=CARTESIAN_POINT('Ctrl Pts',(1.61006596901441,5.79737396808312,-7.83630573519319));
#6738=CARTESIAN_POINT('Ctrl Pts',(1.61006596901441,6.20262603191688,-7.83630573519319));
#6739=CARTESIAN_POINT('Ctrl Pts',(1.5693348410951,6.41832103026994,-7.84501220025286));
#6740=CARTESIAN_POINT('Ctrl Pts',(1.40458789962237,6.81433761606399,-7.876176798428));
#6741=CARTESIAN_POINT('Ctrl Pts',(1.28060364728793,6.99470995245198,-7.89815501897568));
#6742=CARTESIAN_POINT('Ctrl Pts',(0.995172181265423,7.27930851128247,-7.93916938835585));
#6743=CARTESIAN_POINT('Ctrl Pts',(0.814524503839801,7.4027416231449,-7.96090747080436));
#6744=CARTESIAN_POINT('Ctrl Pts',(0.418224335279089,7.56667303463175,-7.99153216392396));
#6745=CARTESIAN_POINT('Ctrl Pts',(0.202527815380415,7.60714285714286,-8.));
#6746=CARTESIAN_POINT('Ctrl Pts',(-0.202527815380416,7.60714285714286,-8.));
#6747=CARTESIAN_POINT('Ctrl Pts',(-0.41822433527909,7.56667303463175,-7.99153216392396));
#6748=CARTESIAN_POINT('Ctrl Pts',(-0.814524503839802,7.4027416231449,-7.96090747080436));
#6749=CARTESIAN_POINT('Ctrl Pts',(-0.995172181265423,7.27930851128247,-7.93916938835585));
#6750=CARTESIAN_POINT('Ctrl Pts',(-1.28060364728793,6.99470995245198,-7.89815501897568));
#6751=CARTESIAN_POINT('Ctrl Pts',(-1.40458789962237,6.81433761606399,-7.876176798428));
#6752=CARTESIAN_POINT('Ctrl Pts',(-1.5693348410951,6.41832103026994,-7.84501220025286));
#6753=CARTESIAN_POINT('Ctrl Pts',(-1.61006596901441,6.20262603191688,-7.83630573519319));
#6754=CARTESIAN_POINT('Ctrl Pts',(-1.61006596901441,6.,-7.83630573519319));
#6755=CARTESIAN_POINT('Ctrl Pts',(-1.61006596901441,6.,-7.83630573519319));
#6756=CARTESIAN_POINT('Ctrl Pts',(-1.61006596901441,5.79737396808312,-7.83630573519319));
#6757=CARTESIAN_POINT('Ctrl Pts',(-1.5693348410951,5.58167896973006,-7.84501220025286));
#6758=CARTESIAN_POINT('Ctrl Pts',(-1.41259784295971,5.2049165830398,-7.87466158568243));
#6759=CARTESIAN_POINT('Ctrl Pts',(-1.30457569943121,5.04029901068342,-7.89393477892562));
#6760=CARTESIAN_POINT('Ctrl Pts',(-1.17898168752143,4.90550167217474,-7.91264824066438));
#6761=CARTESIAN_POINT('Origin',(0.,6.,14.));
#6762=CARTESIAN_POINT('',(-2.,6.,14.));
#6763=CARTESIAN_POINT('Origin',(0.,6.,14.));
#6764=CARTESIAN_POINT('',(-2.,6.,14.));
#6765=CARTESIAN_POINT('',(0.,0.,0.));
#6766=CARTESIAN_POINT('Origin',(0.,0.,0.));
#6767=CARTESIAN_POINT('',(28.,0.,2.));
#6768=CARTESIAN_POINT('Origin',(28.,0.,0.));
#6769=CARTESIAN_POINT('',(0.,0.,1.5));
#6770=CARTESIAN_POINT('',(0.,-1.83697019872103E-16,1.5));
#6771=CARTESIAN_POINT('Origin',(0.,0.,0.));
#6772=CARTESIAN_POINT('Origin',(27.9999999999979,-2.,0.));
#6773=CARTESIAN_POINT('Origin',(-1.14810637420064E-16,0.,0.));
#6774=CARTESIAN_POINT('',(0.,0.,0.));
#6775=CARTESIAN_POINT('Origin',(25.9999999999979,50.,0.));
#6776=CARTESIAN_POINT('',(-25.9999999999982,49.9999999999998,-3.18408167778287E-15));
#6777=CARTESIAN_POINT('Origin',(-1.71512449944288E-13,49.9999999999998,
0.));
#6778=CARTESIAN_POINT('',(-18.0000000000003,49.9999999999998,-2.20436423846525E-15));
#6779=CARTESIAN_POINT('Origin',(-1.71512449944288E-13,49.9999999999998,
0.));
#6780=CARTESIAN_POINT('Origin',(2.05611259281969E-12,-599.406221964517,
0.));
#6781=CARTESIAN_POINT('',(-18.0000000000001,3.99999999999984,-2.20436423846525E-15));
#6782=CARTESIAN_POINT('',(-17.999999999998,-599.406221964517,-2.20436423846525E-15));
#6783=CARTESIAN_POINT('',(18.,3.99999999999995,0.));
#6784=CARTESIAN_POINT('Origin',(-1.37209959955424E-14,3.99999999999989,
0.));
#6785=CARTESIAN_POINT('Origin',(-1.37209959955424E-14,3.99999999999989,
0.));
#6786=CARTESIAN_POINT('Origin',(-1.37209959955424E-14,3.99999999999989,
0.));
#6787=CARTESIAN_POINT('',(10.,3.43024899888577E-14,0.));
#6788=CARTESIAN_POINT('',(-9.99999999999995,0.,-1.22464679914735E-15));
#6789=CARTESIAN_POINT('Origin',(0.,0.,0.));
#6790=CARTESIAN_POINT('Origin',(0.,0.,0.));
#6791=CARTESIAN_POINT('',(18.,3.99999999999995,-2.20436423846524E-15));
#6792=CARTESIAN_POINT('Origin',(2.05611259281969E-12,-599.406221964517,
0.));
#6793=CARTESIAN_POINT('',(-9.99999999999985,-30.0000000000001,-1.22464679914735E-15));
#6794=CARTESIAN_POINT('',(-9.99999999999789,-599.406221964517,-1.22464679914735E-15));
#6795=CARTESIAN_POINT('Origin',(1.02907469966573E-13,-30.,0.));
#6796=CARTESIAN_POINT('Origin',(10.,-30.,0.));
#6797=CARTESIAN_POINT('',(20.,-30.0000000000001,0.));
#6798=CARTESIAN_POINT('Origin',(1.02907469966574E-13,-30.0000000000001,
0.));
#6799=CARTESIAN_POINT('Origin',(1.02907469966574E-13,-30.0000000000001,
0.));
#6800=CARTESIAN_POINT('',(28.,-4.00000000000002,0.));
#6801=CARTESIAN_POINT('Origin',(1.37209959955436E-14,-4.00000000000011,
0.));
#6802=CARTESIAN_POINT('',(20.,-30.0000000000001,-2.44929359829469E-15));
#6803=CARTESIAN_POINT('Origin',(28.,-4.00000000000002,0.));
#6804=CARTESIAN_POINT('',(-40.,-4.00000000000027,-4.89858719658941E-15));
#6805=CARTESIAN_POINT('Origin',(1.37209959955436E-14,-4.00000000000011,
0.));
#6806=CARTESIAN_POINT('Origin',(2.05611259281969E-12,-599.406221964517,
0.));
#6807=CARTESIAN_POINT('',(-40.,3.99999999999977,-4.89858719658941E-15));
#6808=CARTESIAN_POINT('',(-39.9999999999979,-599.406221964517,-4.89858719658941E-15));
#6809=CARTESIAN_POINT('Origin',(-1.37209959955424E-14,3.99999999999989,
0.));
#6810=CARTESIAN_POINT('Origin',(40.,3.99999999999992,0.));
#6811=CARTESIAN_POINT('',(-89.999999999998,3.99999999999935,-1.10218211923259E-14));
#6812=CARTESIAN_POINT('Origin',(-1.37209959955416E-14,3.99999999999967,
0.));
#6813=CARTESIAN_POINT('',(-64.,3.99999999999956,-2.44403693719019E-13));
#6814=CARTESIAN_POINT('Origin',(-70.,3.99999999999954,-2.44403693719019E-13));
#6815=CARTESIAN_POINT('',(5.99999999999999,3.9999999999998,-70.));
#6816=CARTESIAN_POINT('Origin',(-1.37209959955424E-14,3.99999999999978,
-70.));
#6817=CARTESIAN_POINT('',(76.,4.00000000000004,7.33211081157058E-13));
#6818=CARTESIAN_POINT('Origin',(70.,4.00000000000002,7.33211081157058E-13));
#6819=CARTESIAN_POINT('',(5.99999999999999,3.9999999999998,70.));
#6820=CARTESIAN_POINT('Origin',(-1.37209959955423E-14,3.99999999999978,
70.));
#6821=CARTESIAN_POINT('Origin',(2.05611259281969E-12,-599.406221964517,
0.));
#6822=CARTESIAN_POINT('',(-89.999999999998,19.9999999999994,-1.10218211923259E-14));
#6823=CARTESIAN_POINT('',(-89.9999999999959,-599.406221964518,-1.10218211923259E-14));
#6824=CARTESIAN_POINT('Origin',(-6.86049799777142E-14,19.9999999999997,
0.));
#6825=CARTESIAN_POINT('Origin',(89.9999999999979,20.0000000000001,0.));
#6826=CARTESIAN_POINT('',(-64.0000000000001,19.9999999999996,-2.45138481798508E-13));
#6827=CARTESIAN_POINT('Origin',(-70.0000000000001,19.9999999999996,-2.44403693719019E-13));
#6828=CARTESIAN_POINT('',(5.99999999999993,19.9999999999998,-70.));
#6829=CARTESIAN_POINT('Origin',(-6.86049799777149E-14,19.9999999999998,
-70.));
#6830=CARTESIAN_POINT('',(76.,20.0000000000001,7.3247629307757E-13));
#6831=CARTESIAN_POINT('Origin',(69.9999999999999,20.,7.33211081157058E-13));
#6832=CARTESIAN_POINT('',(5.99999999999993,19.9999999999998,70.));
#6833=CARTESIAN_POINT('Origin',(-6.86049799777146E-14,19.9999999999998,
70.));
#6834=CARTESIAN_POINT('',(-25.9999999999981,19.9999999999998,-3.18408167778287E-15));
#6835=CARTESIAN_POINT('Origin',(-6.86049799777149E-14,19.9999999999999,
0.));
#6836=CARTESIAN_POINT('Origin',(2.05611259281969E-12,-599.406221964517,
0.));
#6837=CARTESIAN_POINT('',(-25.9999999999959,-599.406221964517,-3.18408167778287E-15));
#6838=CARTESIAN_POINT('Origin',(1.02907469966574E-13,-30.0000000000004,
70.));
#6839=CARTESIAN_POINT('',(6.0000000000001,-30.0000000000004,70.));
#6840=CARTESIAN_POINT('Origin',(70.0000000000001,-30.0000000000001,7.33211081157058E-13));
#6841=CARTESIAN_POINT('',(76.0000000000001,-30.0000000000001,7.3247629307757E-13));
#6842=CARTESIAN_POINT('Origin',(1.02907469966575E-13,-30.0000000000004,
-70.));
#6843=CARTESIAN_POINT('',(6.0000000000001,-30.0000000000004,-70.));
#6844=CARTESIAN_POINT('Origin',(-69.9999999999999,-30.0000000000006,-2.4440369371902E-13));
#6845=CARTESIAN_POINT('',(-63.9999999999999,-30.0000000000006,-2.45138481798508E-13));
#6846=CARTESIAN_POINT('',(0.,0.,0.));
#6847=CARTESIAN_POINT('Origin',(1.66027257158657E-12,-484.009345130884,
0.));
#6848=CARTESIAN_POINT('',(-10.0000000000001,18.,-1.22464679914736E-15));
#6849=CARTESIAN_POINT('Origin',(-6.17444819799439E-14,18.,0.));
#6850=CARTESIAN_POINT('',(-10.0000000000001,3.99999999999991,-1.22464679914736E-15));
#6851=CARTESIAN_POINT('',(-9.99999999999839,-484.009345130884,-1.22464679914736E-15));
#6852=CARTESIAN_POINT('Origin',(-1.37209959955432E-14,3.99999999999995,
0.));
#6853=CARTESIAN_POINT('Origin',(10.,18.,0.));
#6854=CARTESIAN_POINT('',(-22.0000000000001,17.9999999999998,-2.69422295812418E-15));
#6855=CARTESIAN_POINT('Origin',(-6.17444819799435E-14,17.9999999999999,
0.));
#6856=CARTESIAN_POINT('Origin',(1.66027257158657E-12,-484.009345130884,
0.));
#6857=CARTESIAN_POINT('',(-22.0000000000001,15.9999999999998,-2.69422295812418E-15));
#6858=CARTESIAN_POINT('Origin',(-5.48839839821719E-14,15.9999999999998,
0.));
#6859=CARTESIAN_POINT('',(-21.9999999999984,-484.009345130884,-2.69422295812418E-15));
#6860=CARTESIAN_POINT('Origin',(22.,16.,0.));
#6861=CARTESIAN_POINT('',(-18.0000000000001,15.9999999999998,-2.20436423846524E-15));
#6862=CARTESIAN_POINT('Origin',(-5.48839839821719E-14,15.9999999999998,
0.));
#6863=CARTESIAN_POINT('Origin',(1.66027257158657E-12,-484.009345130884,
0.));
#6864=CARTESIAN_POINT('',(-18.,-1.4210854715202E-13,-2.20436423846524E-15));
#6865=CARTESIAN_POINT('Origin',(0.,-5.55111512312578E-14,0.));
#6866=CARTESIAN_POINT('',(-17.9999999999984,-484.009345130884,-2.20436423846524E-15));
#6867=CARTESIAN_POINT('Origin',(-1.37209959955432E-14,3.99999999999995,
0.));
#6868=CARTESIAN_POINT('',(-10.,3.99999999999991,-1.22464679914736E-15));
#6869=CARTESIAN_POINT('',(0.,0.,0.));
#6870=CARTESIAN_POINT('Origin',(20.0000000000004,40.,34.6410161513773));
#6871=CARTESIAN_POINT('',(40.,34.6410161513776,-1.04083408558608E-14));
#6872=CARTESIAN_POINT('',(40.,0.,0.));
#6873=CARTESIAN_POINT('',(40.,34.6410161513776,0.));
#6874=CARTESIAN_POINT('',(30.0000000000001,40.,17.3205080756886));
#6875=CARTESIAN_POINT('Ctrl Pts',(40.,34.6410161513776,-8.88178419700125E-15));
#6876=CARTESIAN_POINT('Ctrl Pts',(40.,34.8675563853847,-8.94780562024841E-15));
#6877=CARTESIAN_POINT('Ctrl Pts',(39.9845496882855,35.1132553852053,0.0267607248823537));
#6878=CARTESIAN_POINT('Ctrl Pts',(39.9209089392646,35.5879596782423,0.136989735618295));
#6879=CARTESIAN_POINT('Ctrl Pts',(39.8729336465118,35.8170802394984,0.22008538017415));
#6880=CARTESIAN_POINT('Ctrl Pts',(39.7450039767544,36.292215920861,0.44166606798931));
#6881=CARTESIAN_POINT('Ctrl Pts',(39.6445377014013,36.5686663529566,0.615678761348116));
#6882=CARTESIAN_POINT('Ctrl Pts',(39.413570269859,37.0692605098588,1.01572608767312));
#6883=CARTESIAN_POINT('Ctrl Pts',(39.2834488566673,37.2941045349873,1.24110298647387));
#6884=CARTESIAN_POINT('Ctrl Pts',(38.9479833579045,37.7957977176563,1.82214627451743));
#6885=CARTESIAN_POINT('Ctrl Pts',(38.6995716833136,38.0825278600404,2.25240791610222));
#6886=CARTESIAN_POINT('Ctrl Pts',(38.1796891744627,38.5640991767506,3.15287083539827));
#6887=CARTESIAN_POINT('Ctrl Pts',(37.9085074292358,38.7601877193308,3.62257139621652));
#6888=CARTESIAN_POINT('Ctrl Pts',(37.077311811023,39.2690611683488,5.06224443798978));
#6889=CARTESIAN_POINT('Ctrl Pts',(36.4597275654282,39.4955705648851,6.13193172931402));
#6890=CARTESIAN_POINT('Ctrl Pts',(35.1851649957381,39.8044631544014,8.33953885744289));
#6891=CARTESIAN_POINT('Ctrl Pts',(34.5280891925476,39.885235330521,9.47762753299292));
#6892=CARTESIAN_POINT('Ctrl Pts',(33.2073007717862,39.9780696179776,11.7653001838004));
#6893=CARTESIAN_POINT('Ctrl Pts',(32.5438367467531,39.9905745886849,12.9144535841519));
#6894=CARTESIAN_POINT('Ctrl Pts',(31.2436555254328,40.001470043377,15.1664335185256));
#6895=CARTESIAN_POINT('Ctrl Pts',(30.6069386222742,40.,16.2692595448342));
#6896=CARTESIAN_POINT('Ctrl Pts',(30.0000000000002,40.,17.3205080756887));
#6897=CARTESIAN_POINT('',(20.0000000000004,34.6410161513776,34.6410161513773));
#6898=CARTESIAN_POINT('Ctrl Pts',(30.0000000000002,40.,17.3205080756887));
#6899=CARTESIAN_POINT('Ctrl Pts',(29.3930613777262,40.,18.3717566065431));
#6900=CARTESIAN_POINT('Ctrl Pts',(28.7563444745676,40.001470043377,19.4745826328517));
#6901=CARTESIAN_POINT('Ctrl Pts',(27.4561632532473,39.990574588685,21.7265625672254));
#6902=CARTESIAN_POINT('Ctrl Pts',(26.7926992282142,39.9780696179776,22.8757159675769));
#6903=CARTESIAN_POINT('Ctrl Pts',(25.4719108074528,39.885235330521,25.1633886183844));
#6904=CARTESIAN_POINT('Ctrl Pts',(24.8148350042623,39.8044631544014,26.3014772939344));
#6905=CARTESIAN_POINT('Ctrl Pts',(23.5402724345722,39.4955705648851,28.5090844220633));
#6906=CARTESIAN_POINT('Ctrl Pts',(22.9226881889774,39.2690611683488,29.5787717133875));
#6907=CARTESIAN_POINT('Ctrl Pts',(22.0914925707646,38.7601877193308,31.0184447551608));
#6908=CARTESIAN_POINT('Ctrl Pts',(21.8203108255377,38.5640991767506,31.4881453159791));
#6909=CARTESIAN_POINT('Ctrl Pts',(21.3004283166868,38.0825278600404,32.3886082352751));
#6910=CARTESIAN_POINT('Ctrl Pts',(21.0520166420959,37.7957977176563,32.8188698768599));
#6911=CARTESIAN_POINT('Ctrl Pts',(20.7165511433331,37.2941045349873,33.3999131649034));
#6912=CARTESIAN_POINT('Ctrl Pts',(20.5864297301414,37.0692605098588,33.6252900637042));
#6913=CARTESIAN_POINT('Ctrl Pts',(20.3554622985991,36.5686663529566,34.0253373900292));
#6914=CARTESIAN_POINT('Ctrl Pts',(20.2549960232459,36.292215920861,34.199350083388));
#6915=CARTESIAN_POINT('Ctrl Pts',(20.1270663534886,35.8170802394984,34.4209307712032));
#6916=CARTESIAN_POINT('Ctrl Pts',(20.0790910607358,35.5879596782423,34.504026415759));
#6917=CARTESIAN_POINT('Ctrl Pts',(20.0154503117149,35.1132553852053,34.614255426495));
#6918=CARTESIAN_POINT('Ctrl Pts',(20.0000000000004,34.8675563853847,34.6410161513773));
#6919=CARTESIAN_POINT('Ctrl Pts',(20.0000000000004,34.6410161513776,34.6410161513773));
#6920=CARTESIAN_POINT('',(20.0000000000004,0.,34.6410161513773));
#6921=CARTESIAN_POINT('',(20.0000000000004,34.6410161513776,34.6410161513773));
#6922=CARTESIAN_POINT('',(20.0000000000004,0.,34.6410161513773));
#6923=CARTESIAN_POINT('Origin',(40.,40.,0.));
#6924=CARTESIAN_POINT('',(19.9999999999999,34.6410161513776,-34.6410161513776));
#6925=CARTESIAN_POINT('',(19.9999999999999,0.,-34.6410161513776));
#6926=CARTESIAN_POINT('',(19.9999999999999,34.6410161513776,-34.6410161513776));
#6927=CARTESIAN_POINT('',(30.,40.,-17.3205080756888));
#6928=CARTESIAN_POINT('Ctrl Pts',(19.9999999999999,34.6410161513776,-34.6410161513776));
#6929=CARTESIAN_POINT('Ctrl Pts',(19.9999999999999,34.9287398464594,-34.6410161513776));
#6930=CARTESIAN_POINT('Ctrl Pts',(20.0296992577666,35.2688605719923,-34.5895755279786));
#6931=CARTESIAN_POINT('Ctrl Pts',(20.1304657002358,35.8569297033293,-34.4150429299239));
#6932=CARTESIAN_POINT('Ctrl Pts',(20.2276726156403,36.2073107797085,-34.2466756135964));
#6933=CARTESIAN_POINT('Ctrl Pts',(20.4872196510673,36.9022698032704,-33.7971269612829));
#6934=CARTESIAN_POINT('Ctrl Pts',(20.7008503712725,37.2910923293497,-33.4271076998299));
#6935=CARTESIAN_POINT('Ctrl Pts',(21.1750144218796,37.9485573400285,-32.6058314730557));
#6936=CARTESIAN_POINT('Ctrl Pts',(21.4351301137511,38.2184038124865,-32.1552978788883));
#6937=CARTESIAN_POINT('Ctrl Pts',(22.2930459787064,38.9613500039003,-30.6693440121665));
#6938=CARTESIAN_POINT('Ctrl Pts',(22.9545391795447,39.2795989494824,-29.5236041794531));
#6939=CARTESIAN_POINT('Ctrl Pts',(24.3278859649791,39.7200338827688,-27.1448977706694));
#6940=CARTESIAN_POINT('Ctrl Pts',(25.0403210919701,39.8349356144784,-25.9109239336242));
#6941=CARTESIAN_POINT('Ctrl Pts',(26.4795724684824,39.9680208314247,-23.4180674246415));
#6942=CARTESIAN_POINT('Ctrl Pts',(27.2055367776954,39.986280068449,-22.1606603566028));
#6943=CARTESIAN_POINT('Ctrl Pts',(28.6316842828226,40.0021234610802,-19.690500418635));
#6944=CARTESIAN_POINT('Ctrl Pts',(29.3318666629522,40.,-18.477748961686));
#6945=CARTESIAN_POINT('Ctrl Pts',(30.,40.,-17.3205080756888));
#6946=CARTESIAN_POINT('Ctrl Pts',(30.,40.,-17.3205080756888));
#6947=CARTESIAN_POINT('Ctrl Pts',(30.6681333370477,40.,-16.1632671896916));
#6948=CARTESIAN_POINT('Ctrl Pts',(31.3683157171773,40.0021234610802,-14.9505157327426));
#6949=CARTESIAN_POINT('Ctrl Pts',(32.7944632223045,39.986280068449,-12.4803557947748));
#6950=CARTESIAN_POINT('Ctrl Pts',(33.5204275315175,39.9680208314247,-11.2229487267361));
#6951=CARTESIAN_POINT('Ctrl Pts',(34.9596789080298,39.8349356144784,-8.73009221775341));
#6952=CARTESIAN_POINT('Ctrl Pts',(35.6721140350208,39.7200338827688,-7.4961183807082));
#6953=CARTESIAN_POINT('Ctrl Pts',(37.0454608204552,39.2795989494824,-5.11741197192452));
#6954=CARTESIAN_POINT('Ctrl Pts',(37.7069540212935,38.9613500039003,-3.97167213921113));
#6955=CARTESIAN_POINT('Ctrl Pts',(38.5648698862487,38.2184038124865,-2.48571827248925));
#6956=CARTESIAN_POINT('Ctrl Pts',(38.8249855781203,37.9485573400285,-2.03518467832188));
#6957=CARTESIAN_POINT('Ctrl Pts',(39.2991496287274,37.2910923293497,-1.21390845154769));
#6958=CARTESIAN_POINT('Ctrl Pts',(39.5127803489326,36.9022698032704,-0.843889190094687));
#6959=CARTESIAN_POINT('Ctrl Pts',(39.7723273843596,36.2073107797085,-0.394340537781235));
#6960=CARTESIAN_POINT('Ctrl Pts',(39.8695342997641,35.8569297033293,-0.225973221453679));
#6961=CARTESIAN_POINT('Ctrl Pts',(39.9703007422333,35.2688605719923,-0.0514406233989685));
#6962=CARTESIAN_POINT('Ctrl Pts',(40.,34.9287398464594,-6.24836289329261E-15));
#6963=CARTESIAN_POINT('Ctrl Pts',(40.,34.6410161513776,-6.66133814775094E-15));
#6964=CARTESIAN_POINT('',(40.,0.,0.));
#6965=CARTESIAN_POINT('Origin',(19.9999999999999,40.,-34.6410161513776));
#6966=CARTESIAN_POINT('',(-20.0000000000002,34.6410161513776,-34.6410161513774));
#6967=CARTESIAN_POINT('',(-1.14175909504024E-13,40.,-34.6410161513776));
#6968=CARTESIAN_POINT('Ctrl Pts',(-20.0000000000001,34.6410161513776,-34.6410161513775));
#6969=CARTESIAN_POINT('Ctrl Pts',(-20.0000000000001,34.9287398464594,-34.6410161513775));
#6970=CARTESIAN_POINT('Ctrl Pts',(-19.9406014844668,35.2688605719923,-34.6410161513775));
#6971=CARTESIAN_POINT('Ctrl Pts',(-19.7390685995283,35.8569297033293,-34.6410161513775));
#6972=CARTESIAN_POINT('Ctrl Pts',(-19.5446547687194,36.2073107797085,-34.6410161513775));
#6973=CARTESIAN_POINT('Ctrl Pts',(-19.0255606978654,36.9022698032704,-34.6410161513775));
#6974=CARTESIAN_POINT('Ctrl Pts',(-18.5982992574549,37.2910923293497,-34.6410161513775));
#6975=CARTESIAN_POINT('Ctrl Pts',(-17.6499711562407,37.9485573400285,-34.6410161513775));
#6976=CARTESIAN_POINT('Ctrl Pts',(-17.1297397724977,38.2184038124865,-34.6410161513775));
#6977=CARTESIAN_POINT('Ctrl Pts',(-15.4139080425872,38.9613500039003,-34.6410161513775));
#6978=CARTESIAN_POINT('Ctrl Pts',(-14.0909216409105,39.2795989494824,-34.6410161513775));
#6979=CARTESIAN_POINT('Ctrl Pts',(-11.3442280700418,39.7200338827688,-34.6410161513775));
#6980=CARTESIAN_POINT('Ctrl Pts',(-9.91935781605978,39.8349356144784,-34.6410161513775));
#6981=CARTESIAN_POINT('Ctrl Pts',(-7.0408550630352,39.9680208314247,-34.6410161513775));
#6982=CARTESIAN_POINT('Ctrl Pts',(-5.5889264446091,39.986280068449,-34.6410161513775));
#6983=CARTESIAN_POINT('Ctrl Pts',(-2.73663143435478,40.0021234610802,-34.6410161513775));
#6984=CARTESIAN_POINT('Ctrl Pts',(-1.33626667409561,40.,-34.6410161513775));
#6985=CARTESIAN_POINT('Ctrl Pts',(-1.14175909504024E-13,40.,-34.6410161513775));
#6986=CARTESIAN_POINT('Ctrl Pts',(-1.13797860024079E-13,40.,-34.6410161513775));
#6987=CARTESIAN_POINT('Ctrl Pts',(1.33626667409539,40.,-34.6410161513775));
#6988=CARTESIAN_POINT('Ctrl Pts',(2.73663143435455,40.0021234610802,-34.6410161513775));
#6989=CARTESIAN_POINT('Ctrl Pts',(5.58892644460887,39.986280068449,-34.6410161513775));
#6990=CARTESIAN_POINT('Ctrl Pts',(7.04085506303497,39.9680208314247,-34.6410161513775));
#6991=CARTESIAN_POINT('Ctrl Pts',(9.91935781605956,39.8349356144784,-34.6410161513776));
#6992=CARTESIAN_POINT('Ctrl Pts',(11.3442280700416,39.7200338827688,-34.6410161513776));
#6993=CARTESIAN_POINT('Ctrl Pts',(14.0909216409102,39.2795989494824,-34.6410161513776));
#6994=CARTESIAN_POINT('Ctrl Pts',(15.413908042587,38.9613500039003,-34.6410161513776));
#6995=CARTESIAN_POINT('Ctrl Pts',(17.1297397724974,38.2184038124865,-34.6410161513776));
#6996=CARTESIAN_POINT('Ctrl Pts',(17.6499711562404,37.9485573400285,-34.6410161513776));
#6997=CARTESIAN_POINT('Ctrl Pts',(18.5982992574547,37.2910923293498,-34.6410161513776));
#6998=CARTESIAN_POINT('Ctrl Pts',(19.0255606978652,36.9022698032704,-34.6410161513776));
#6999=CARTESIAN_POINT('Ctrl Pts',(19.5446547687192,36.2073107797085,-34.6410161513776));
#7000=CARTESIAN_POINT('Ctrl Pts',(19.7390685995281,35.8569297033293,-34.6410161513776));
#7001=CARTESIAN_POINT('Ctrl Pts',(19.9406014844666,35.2688605719923,-34.6410161513776));
#7002=CARTESIAN_POINT('Ctrl Pts',(19.9999999999999,34.9287398464594,-34.6410161513776));
#7003=CARTESIAN_POINT('Ctrl Pts',(19.9999999999999,34.6410161513776,-34.6410161513776));
#7004=CARTESIAN_POINT('',(-20.0000000000001,0.,-34.6410161513775));
#7005=CARTESIAN_POINT('',(19.9999999999999,0.,-34.6410161513776));
#7006=CARTESIAN_POINT('',(-20.0000000000001,34.6410161513776,-34.6410161513775));
#7007=CARTESIAN_POINT('Origin',(-20.0000000000001,40.,-34.6410161513775));
#7008=CARTESIAN_POINT('',(-40.,34.6410161513776,2.84494650060196E-13));
#7009=CARTESIAN_POINT('',(-40.,0.,2.79318507107451E-13));
#7010=CARTESIAN_POINT('',(-40.,34.6410161513776,2.79318507107451E-13));
#7011=CARTESIAN_POINT('',(-30.0000000000001,40.,-17.3205080756886));
#7012=CARTESIAN_POINT('Ctrl Pts',(-40.,34.6410161513776,3.10862446895044E-13));
#7013=CARTESIAN_POINT('Ctrl Pts',(-40.,34.9287398464594,3.11261743733806E-13));
#7014=CARTESIAN_POINT('Ctrl Pts',(-39.9703007422333,35.2688605719923,-0.0514406233986507));
#7015=CARTESIAN_POINT('Ctrl Pts',(-39.8695342997641,35.8569297033293,-0.225973221453362));
#7016=CARTESIAN_POINT('Ctrl Pts',(-39.7723273843596,36.2073107797085,-0.394340537780919));
#7017=CARTESIAN_POINT('Ctrl Pts',(-39.5127803489326,36.9022698032704,-0.843889190094373));
#7018=CARTESIAN_POINT('Ctrl Pts',(-39.2991496287274,37.2910923293497,-1.21390845154738));
#7019=CARTESIAN_POINT('Ctrl Pts',(-38.8249855781203,37.9485573400285,-2.03518467832158));
#7020=CARTESIAN_POINT('Ctrl Pts',(-38.5648698862488,38.2184038124865,-2.48571827248894));
#7021=CARTESIAN_POINT('Ctrl Pts',(-37.7069540212935,38.9613500039003,-3.97167213921083));
#7022=CARTESIAN_POINT('Ctrl Pts',(-37.0454608204552,39.2795989494824,-5.11741197192423));
#7023=CARTESIAN_POINT('Ctrl Pts',(-35.6721140350209,39.7200338827688,-7.49611838070793));
#7024=CARTESIAN_POINT('Ctrl Pts',(-34.9596789080299,39.8349356144784,-8.73009221775313));
#7025=CARTESIAN_POINT('Ctrl Pts',(-33.5204275315176,39.9680208314247,-11.2229487267359));
#7026=CARTESIAN_POINT('Ctrl Pts',(-32.7944632223045,39.986280068449,-12.4803557947745));
#7027=CARTESIAN_POINT('Ctrl Pts',(-31.3683157171774,40.0021234610802,-14.9505157327424));
#7028=CARTESIAN_POINT('Ctrl Pts',(-30.6681333370478,40.,-16.1632671896913));
#7029=CARTESIAN_POINT('Ctrl Pts',(-30.0000000000001,40.,-17.3205080756886));
#7030=CARTESIAN_POINT('Ctrl Pts',(-30.0000000000001,40.,-17.3205080756886));
#7031=CARTESIAN_POINT('Ctrl Pts',(-29.3318666629523,40.,-18.4777489616858));
#7032=CARTESIAN_POINT('Ctrl Pts',(-28.6316842828228,40.0021234610802,-19.6905004186348));
#7033=CARTESIAN_POINT('Ctrl Pts',(-27.2055367776956,39.986280068449,-22.1606603566026));
#7034=CARTESIAN_POINT('Ctrl Pts',(-26.4795724684826,39.9680208314247,-23.4180674246413));
#7035=CARTESIAN_POINT('Ctrl Pts',(-25.0403210919703,39.8349356144784,-25.910923933624));
#7036=CARTESIAN_POINT('Ctrl Pts',(-24.3278859649793,39.7200338827688,-27.1448977706692));
#7037=CARTESIAN_POINT('Ctrl Pts',(-22.9545391795449,39.2795989494824,-29.5236041794529));
#7038=CARTESIAN_POINT('Ctrl Pts',(-22.2930459787066,38.9613500039003,-30.6693440121663));
#7039=CARTESIAN_POINT('Ctrl Pts',(-21.4351301137514,38.2184038124865,-32.1552978788882));
#7040=CARTESIAN_POINT('Ctrl Pts',(-21.1750144218799,37.9485573400285,-32.6058314730556));
#7041=CARTESIAN_POINT('Ctrl Pts',(-20.7008503712728,37.2910923293497,-33.4271076998298));
#7042=CARTESIAN_POINT('Ctrl Pts',(-20.4872196510675,36.9022698032704,-33.7971269612828));
#7043=CARTESIAN_POINT('Ctrl Pts',(-20.2276726156405,36.2073107797085,-34.2466756135962));
#7044=CARTESIAN_POINT('Ctrl Pts',(-20.1304657002361,35.8569297033293,-34.4150429299238));
#7045=CARTESIAN_POINT('Ctrl Pts',(-20.0296992577668,35.2688605719923,-34.5895755279785));
#7046=CARTESIAN_POINT('Ctrl Pts',(-20.0000000000001,34.9287398464594,-34.6410161513775));
#7047=CARTESIAN_POINT('Ctrl Pts',(-20.0000000000001,34.6410161513776,-34.6410161513775));
#7048=CARTESIAN_POINT('',(-20.0000000000001,0.,-34.6410161513775));
#7049=CARTESIAN_POINT('Origin',(-40.,40.,2.79318507107451E-13));
#7050=CARTESIAN_POINT('',(-19.9999999999997,34.6410161513776,34.6410161513777));
#7051=CARTESIAN_POINT('',(-19.9999999999997,0.,34.6410161513777));
#7052=CARTESIAN_POINT('',(-19.9999999999997,34.6410161513776,34.6410161513777));
#7053=CARTESIAN_POINT('',(-29.9999999999999,40.,17.320508075689));
#7054=CARTESIAN_POINT('Ctrl Pts',(-19.9999999999997,34.6410161513776,34.6410161513777));
#7055=CARTESIAN_POINT('Ctrl Pts',(-19.9999999999997,34.9287398464594,34.6410161513777));
#7056=CARTESIAN_POINT('Ctrl Pts',(-20.0296992577664,35.2688605719923,34.5895755279788));
#7057=CARTESIAN_POINT('Ctrl Pts',(-20.1304657002356,35.8569297033293,34.4150429299241));
#7058=CARTESIAN_POINT('Ctrl Pts',(-20.2276726156401,36.2073107797085,34.2466756135965));
#7059=CARTESIAN_POINT('Ctrl Pts',(-20.4872196510671,36.9022698032704,33.797126961283));
#7060=CARTESIAN_POINT('Ctrl Pts',(-20.7008503712723,37.2910923293498,33.4271076998301));
#7061=CARTESIAN_POINT('Ctrl Pts',(-21.1750144218794,37.9485573400285,32.6058314730559));
#7062=CARTESIAN_POINT('Ctrl Pts',(-21.4351301137509,38.2184038124865,32.1552978788885));
#7063=CARTESIAN_POINT('Ctrl Pts',(-22.2930459787062,38.9613500039003,30.6693440121666));
#7064=CARTESIAN_POINT('Ctrl Pts',(-22.9545391795445,39.2795989494824,29.5236041794532));
#7065=CARTESIAN_POINT('Ctrl Pts',(-24.3278859649789,39.7200338827688,27.1448977706696));
#7066=CARTESIAN_POINT('Ctrl Pts',(-25.0403210919699,39.8349356144784,25.9109239336244));
#7067=CARTESIAN_POINT('Ctrl Pts',(-26.4795724684822,39.9680208314247,23.4180674246416));
#7068=CARTESIAN_POINT('Ctrl Pts',(-27.2055367776953,39.986280068449,22.160660356603));
#7069=CARTESIAN_POINT('Ctrl Pts',(-28.6316842828225,40.0021234610802,19.6905004186352));
#7070=CARTESIAN_POINT('Ctrl Pts',(-29.3318666629521,40.,18.4777489616862));
#7071=CARTESIAN_POINT('Ctrl Pts',(-29.9999999999998,40.,17.320508075689));
#7072=CARTESIAN_POINT('Ctrl Pts',(-29.9999999999998,40.,17.320508075689));
#7073=CARTESIAN_POINT('Ctrl Pts',(-30.6681333370476,40.,16.1632671896918));
#7074=CARTESIAN_POINT('Ctrl Pts',(-31.3683157171772,40.0021234610802,14.9505157327428));
#7075=CARTESIAN_POINT('Ctrl Pts',(-32.7944632223044,39.986280068449,12.480355794775));
#7076=CARTESIAN_POINT('Ctrl Pts',(-33.5204275315174,39.9680208314247,11.2229487267364));
#7077=CARTESIAN_POINT('Ctrl Pts',(-34.9596789080297,39.8349356144784,8.73009221775364));
#7078=CARTESIAN_POINT('Ctrl Pts',(-35.6721140350208,39.7200338827688,7.49611838070845));
#7079=CARTESIAN_POINT('Ctrl Pts',(-37.0454608204551,39.2795989494824,5.11741197192477));
#7080=CARTESIAN_POINT('Ctrl Pts',(-37.7069540212935,38.9613500039003,3.97167213921139));
#7081=CARTESIAN_POINT('Ctrl Pts',(-38.5648698862487,38.2184038124865,2.48571827248952));
#7082=CARTESIAN_POINT('Ctrl Pts',(-38.8249855781202,37.9485573400285,2.03518467832214));
#7083=CARTESIAN_POINT('Ctrl Pts',(-39.2991496287274,37.2910923293498,1.21390845154796));
#7084=CARTESIAN_POINT('Ctrl Pts',(-39.5127803489326,36.9022698032704,0.843889190094969));
#7085=CARTESIAN_POINT('Ctrl Pts',(-39.7723273843596,36.2073107797085,0.394340537781517));
#7086=CARTESIAN_POINT('Ctrl Pts',(-39.8695342997641,35.8569297033293,0.225973221453961));
#7087=CARTESIAN_POINT('Ctrl Pts',(-39.9703007422333,35.2688605719923,0.0514406233992506));
#7088=CARTESIAN_POINT('Ctrl Pts',(-40.,34.9287398464594,2.79363226951081E-13));
#7089=CARTESIAN_POINT('Ctrl Pts',(-40.,34.6410161513776,2.79776202205539E-13));
#7090=CARTESIAN_POINT('',(-40.,0.,2.79318507107451E-13));
#7091=CARTESIAN_POINT('Origin',(-19.9999999999997,40.,34.6410161513777));
#7092=CARTESIAN_POINT('',(3.60555503696918E-13,40.,34.6410161513776));
#7093=CARTESIAN_POINT('Ctrl Pts',(20.0000000000004,34.6410161513776,34.6410161513773));
#7094=CARTESIAN_POINT('Ctrl Pts',(20.0000000000004,34.9287398464594,34.6410161513773));
#7095=CARTESIAN_POINT('Ctrl Pts',(19.940601484467,35.2688605719923,34.6410161513773));
#7096=CARTESIAN_POINT('Ctrl Pts',(19.7390685995285,35.8569297033293,34.6410161513773));
#7097=CARTESIAN_POINT('Ctrl Pts',(19.5446547687196,36.2073107797085,34.6410161513773));
#7098=CARTESIAN_POINT('Ctrl Pts',(19.0255606978656,36.9022698032704,34.6410161513773));
#7099=CARTESIAN_POINT('Ctrl Pts',(18.5982992574552,37.2910923293498,34.6410161513773));
#7100=CARTESIAN_POINT('Ctrl Pts',(17.6499711562409,37.9485573400285,34.6410161513773));
#7101=CARTESIAN_POINT('Ctrl Pts',(17.1297397724979,38.2184038124865,34.6410161513773));
#7102=CARTESIAN_POINT('Ctrl Pts',(15.4139080425874,38.9613500039003,34.6410161513774));
#7103=CARTESIAN_POINT('Ctrl Pts',(14.0909216409107,39.2795989494824,34.6410161513774));
#7104=CARTESIAN_POINT('Ctrl Pts',(11.344228070042,39.7200338827688,34.6410161513774));
#7105=CARTESIAN_POINT('Ctrl Pts',(9.91935781606003,39.8349356144784,34.6410161513774));
#7106=CARTESIAN_POINT('Ctrl Pts',(7.04085506303545,39.9680208314247,34.6410161513774));
#7107=CARTESIAN_POINT('Ctrl Pts',(5.58892644460935,39.986280068449,34.6410161513775));
#7108=CARTESIAN_POINT('Ctrl Pts',(2.73663143435502,40.0021234610802,34.6410161513775));
#7109=CARTESIAN_POINT('Ctrl Pts',(1.33626667409586,40.,34.6410161513775));
#7110=CARTESIAN_POINT('Ctrl Pts',(3.60555503696917E-13,40.,34.6410161513775));
#7111=CARTESIAN_POINT('Ctrl Pts',(3.60267371490863E-13,40.,34.6410161513775));
#7112=CARTESIAN_POINT('Ctrl Pts',(-1.33626667409514,40.,34.6410161513775));
#7113=CARTESIAN_POINT('Ctrl Pts',(-2.7366314343543,40.0021234610802,34.6410161513775));
#7114=CARTESIAN_POINT('Ctrl Pts',(-5.58892644460863,39.986280068449,34.6410161513776));
#7115=CARTESIAN_POINT('Ctrl Pts',(-7.04085506303473,39.9680208314247,34.6410161513776));
#7116=CARTESIAN_POINT('Ctrl Pts',(-9.91935781605931,39.8349356144784,34.6410161513776));
#7117=CARTESIAN_POINT('Ctrl Pts',(-11.3442280700413,39.7200338827688,34.6410161513776));
#7118=CARTESIAN_POINT('Ctrl Pts',(-14.09092164091,39.2795989494824,34.6410161513777));
#7119=CARTESIAN_POINT('Ctrl Pts',(-15.4139080425867,38.9613500039003,34.6410161513777));
#7120=CARTESIAN_POINT('Ctrl Pts',(-17.1297397724972,38.2184038124865,34.6410161513777));
#7121=CARTESIAN_POINT('Ctrl Pts',(-17.6499711562402,37.9485573400285,34.6410161513777));
#7122=CARTESIAN_POINT('Ctrl Pts',(-18.5982992574544,37.2910923293498,34.6410161513777));
#7123=CARTESIAN_POINT('Ctrl Pts',(-19.0255606978649,36.9022698032704,34.6410161513777));
#7124=CARTESIAN_POINT('Ctrl Pts',(-19.5446547687189,36.2073107797085,34.6410161513777));
#7125=CARTESIAN_POINT('Ctrl Pts',(-19.7390685995278,35.8569297033293,34.6410161513777));
#7126=CARTESIAN_POINT('Ctrl Pts',(-19.9406014844663,35.2688605719923,34.6410161513777));
#7127=CARTESIAN_POINT('Ctrl Pts',(-19.9999999999997,34.9287398464594,34.6410161513777));
#7128=CARTESIAN_POINT('Ctrl Pts',(-19.9999999999997,34.6410161513776,34.6410161513777));
#7129=CARTESIAN_POINT('',(-19.9999999999997,0.,34.6410161513777));
#7130=CARTESIAN_POINT('Origin',(0.,0.,0.));
#7131=CARTESIAN_POINT('',(-3.18408167778312E-15,0.,26.));
#7132=CARTESIAN_POINT('Origin',(0.,0.,0.));
#7133=CARTESIAN_POINT('Origin',(0.,32.,0.));
#7134=CARTESIAN_POINT('',(-3.18408167778312E-15,32.,26.));
#7135=CARTESIAN_POINT('Origin',(0.,32.,0.));
#7136=CARTESIAN_POINT('',(-3.18408167778312E-15,32.,26.));
#7137=CARTESIAN_POINT('Origin',(0.,32.,0.));
#7138=CARTESIAN_POINT('',(-1.46957615897682E-15,32.,12.));
#7139=CARTESIAN_POINT('Origin',(0.,32.,0.));
#7140=CARTESIAN_POINT('Origin',(0.,34.6410161513776,0.));
#7141=CARTESIAN_POINT('Origin',(0.,40.,0.));
#7142=CARTESIAN_POINT('Origin',(0.,34.6410161513776,0.));
#7143=CARTESIAN_POINT('Origin',(0.,40.,0.));
#7144=CARTESIAN_POINT('Origin',(0.,34.6410161513776,0.));
#7145=CARTESIAN_POINT('Origin',(0.,40.,0.));
#7146=CARTESIAN_POINT('Origin',(0.,34.6410161513776,0.));
#7147=CARTESIAN_POINT('Origin',(0.,40.,0.));
#7148=CARTESIAN_POINT('Origin',(0.,34.6410161513776,0.));
#7149=CARTESIAN_POINT('Origin',(0.,40.,0.));
#7150=CARTESIAN_POINT('Origin',(0.,34.6410161513776,0.));
#7151=CARTESIAN_POINT('Origin',(0.,40.,0.));
#7152=CARTESIAN_POINT('Origin',(0.,96.,0.));
#7153=CARTESIAN_POINT('',(-2.44929359829471E-15,96.,20.));
#7154=CARTESIAN_POINT('Origin',(0.,96.,0.));
#7155=CARTESIAN_POINT('',(-1.22464679914735E-15,96.,-10.));
#7156=CARTESIAN_POINT('Origin',(0.,96.,0.));
#7157=CARTESIAN_POINT('Origin',(0.,40.,0.));
#7158=CARTESIAN_POINT('',(-4.24230095489963E-15,40.,34.6410161513776));
#7159=CARTESIAN_POINT('Origin',(0.,62.,0.));
#7160=CARTESIAN_POINT('',(-1.46957615897682E-15,62.,12.));
#7161=CARTESIAN_POINT('Origin',(0.,62.,0.));
#7162=CARTESIAN_POINT('',(-1.46957615897682E-15,62.,12.));
#7163=CARTESIAN_POINT('Origin',(0.,62.,0.));
#7164=CARTESIAN_POINT('',(0.,62.,-10.));
#7165=CARTESIAN_POINT('Origin',(0.,62.,0.));
#7166=CARTESIAN_POINT('Origin',(0.,0.,0.));
#7167=CARTESIAN_POINT('',(-1.22464679914735E-15,0.,-10.));
#7168=CARTESIAN_POINT('',(0.,0.,0.));
#7169=CARTESIAN_POINT('Origin',(0.,0.,6.));
#7170=CARTESIAN_POINT('',(-5.99999999999999,-16.9705627484771,6.));
#7171=CARTESIAN_POINT('',(-5.99999999999999,-68.1396788547224,6.));
#7172=CARTESIAN_POINT('',(-5.99999999999999,-16.9705627484771,6.));
#7173=CARTESIAN_POINT('',(5.99999617479513,-68.1397016670827,6.00000000000002));
#7174=CARTESIAN_POINT('Ctrl Pts',(-5.99999999999999,-68.1396788547224,6.00000000012849));
#7175=CARTESIAN_POINT('Ctrl Pts',(-5.88220806812114,-68.0712045447482,6.00000000008163));
#7176=CARTESIAN_POINT('Ctrl Pts',(-5.76349611642723,-68.0048909413794,6.00000000005477));
#7177=CARTESIAN_POINT('Ctrl Pts',(-5.64383895277427,-67.9406843861809,6.00000000003867));
#7178=CARTESIAN_POINT('Ctrl Pts',(-5.35720147136636,-67.7868782561497,6.00000000000011));
#7179=CARTESIAN_POINT('Ctrl Pts',(-5.06513993011167,-67.6451640000266,5.99999999998887));
#7180=CARTESIAN_POINT('Ctrl Pts',(-4.76775535283963,-67.5155036880928,6.00000000004808));
#7181=CARTESIAN_POINT('Ctrl Pts',(-4.70882262228595,-67.4898088914871,6.00000000005981));
#7182=CARTESIAN_POINT('Ctrl Pts',(-4.64968086212463,-67.464587446345,6.00000000007612));
#7183=CARTESIAN_POINT('Ctrl Pts',(-4.59033271641865,-67.4398422796416,6.0000000001009));
#7184=CARTESIAN_POINT('Ctrl Pts',(-4.34878747251347,-67.3391301637743,6.00000000020175));
#7185=CARTESIAN_POINT('Ctrl Pts',(-4.10376784428531,-67.2462488735296,6.00000000005394));
#7186=CARTESIAN_POINT('Ctrl Pts',(-3.85528977251545,-67.1613881052392,6.00000000001804));
#7187=CARTESIAN_POINT('Ctrl Pts',(-3.85490034355802,-67.1612551066197,6.00000000001798));
#7188=CARTESIAN_POINT('Ctrl Pts',(-3.8545109061033,-67.1611221277072,6.00000000001793));
#7189=CARTESIAN_POINT('Ctrl Pts',(-3.85412146016043,-67.160989168504,6.00000000001787));
#7190=CARTESIAN_POINT('Ctrl Pts',(-3.60524310476614,-67.0760205908866,5.99999999998215));
#7191=CARTESIAN_POINT('Ctrl Pts',(-3.35289435328196,-66.9991042097109,6.));
#7192=CARTESIAN_POINT('Ctrl Pts',(-3.09960379879075,-66.9308520752212,6.));
#7193=CARTESIAN_POINT('Ctrl Pts',(-3.03719950469825,-66.9140365003897,6.));
#7194=CARTESIAN_POINT('Ctrl Pts',(-2.97470738560379,-66.8977385562704,6.));
#7195=CARTESIAN_POINT('Ctrl Pts',(-2.91216650726521,-66.8819693081272,6.));
#7196=CARTESIAN_POINT('Ctrl Pts',(-2.64202477002678,-66.8138549451454,6.));
#7197=CARTESIAN_POINT('Ctrl Pts',(-2.37097311554184,-66.7556089621424,6.));
#7198=CARTESIAN_POINT('Ctrl Pts',(-2.09860427727656,-66.7069169291021,6.));
#7199=CARTESIAN_POINT('Ctrl Pts',(-2.05141021421883,-66.698479932813,6.));
#7200=CARTESIAN_POINT('Ctrl Pts',(-2.0041766171422,-66.6903296526791,6.));
#7201=CARTESIAN_POINT('Ctrl Pts',(-1.95690138678829,-66.6824642970514,6.));
#7202=CARTESIAN_POINT('Ctrl Pts',(-1.82742310634297,-66.6609225147239,6.));
#7203=CARTESIAN_POINT('Ctrl Pts',(-1.69763250633901,-66.6415181735337,6.));
#7204=CARTESIAN_POINT('Ctrl Pts',(-1.56756922953221,-66.6242591965759,6.));
#7205=CARTESIAN_POINT('Ctrl Pts',(-1.3759989138017,-66.5988384341119,6.));
#7206=CARTESIAN_POINT('Ctrl Pts',(-1.18372985956116,-66.5780591520956,5.99999999999998));
#7207=CARTESIAN_POINT('Ctrl Pts',(-0.990820807203484,-66.5619477872285,
6.00000000000404));
#7208=CARTESIAN_POINT('Ctrl Pts',(-0.667085375757139,-66.5349100738984,
6.00000000001086));
#7209=CARTESIAN_POINT('Ctrl Pts',(-0.341547876894146,-66.5210179927549,
6.00000000002069));
#7210=CARTESIAN_POINT('Ctrl Pts',(-0.0138882729886304,-66.5206865118667,
6.0000000000061));
#7211=CARTESIAN_POINT('Ctrl Pts',(-0.0118363442197238,-66.5206844360076,
6.00000000000601));
#7212=CARTESIAN_POINT('Ctrl Pts',(-0.00978433221009082,-66.5206828919889,
6.00000000000592));
#7213=CARTESIAN_POINT('Ctrl Pts',(-0.00773223806953993,-66.5206818797792,
6.00000000000582));
#7214=CARTESIAN_POINT('Ctrl Pts',(0.223352402590758,-66.5205678956829,5.99999999999557));
#7215=CARTESIAN_POINT('Ctrl Pts',(0.45544978788947,-66.5272104286493,6.));
#7216=CARTESIAN_POINT('Ctrl Pts',(0.686742750504859,-66.5405340810191,6.));
#7217=CARTESIAN_POINT('Ctrl Pts',(0.718187055372043,-66.5423454330911,6.));
#7218=CARTESIAN_POINT('Ctrl Pts',(0.749616505983944,-66.544280190716,6.));
#7219=CARTESIAN_POINT('Ctrl Pts',(0.781026555580905,-66.5463380912692,6.));
#7220=CARTESIAN_POINT('Ctrl Pts',(0.844159742305148,-66.5504744050144,6.));
#7221=CARTESIAN_POINT('Ctrl Pts',(0.907238909031849,-66.5551138190841,5.99999999999562));
#7222=CARTESIAN_POINT('Ctrl Pts',(0.970229312666943,-66.5602532333437,6.00000000002393));
#7223=CARTESIAN_POINT('Ctrl Pts',(1.16909638809118,-66.5764788839859,6.00000000011334));
#7224=CARTESIAN_POINT('Ctrl Pts',(1.36707745106602,-66.5976891098057,6.00000000097192));
#7225=CARTESIAN_POINT('Ctrl Pts',(1.56441901194577,-66.6238225866039,6.0000000005982));
#7226=CARTESIAN_POINT('Ctrl Pts',(1.69159274010741,-66.6406639030476,6.00000000035737));
#7227=CARTESIAN_POINT('Ctrl Pts',(1.81840056742283,-66.6595543873186,6.00000000016109));
#7228=CARTESIAN_POINT('Ctrl Pts',(1.94502307448575,-66.680510813247,6.00000000007684));
#7229=CARTESIAN_POINT('Ctrl Pts',(2.07712304386896,-66.7023737765363,5.99999999998895));
#7230=CARTESIAN_POINT('Ctrl Pts',(2.20902137412523,-66.7264851999825,6.));
#7231=CARTESIAN_POINT('Ctrl Pts',(2.34063577451671,-66.7528468972374,6.));
#7232=CARTESIAN_POINT('Ctrl Pts',(2.51087892012245,-66.7869457363525,6.));
#7233=CARTESIAN_POINT('Ctrl Pts',(2.68076920433902,-66.8248475460883,6.0000000000736));
#7234=CARTESIAN_POINT('Ctrl Pts',(2.84959845041541,-66.8664159843698,6.00000000019824));
#7235=CARTESIAN_POINT('Ctrl Pts',(2.86928581831134,-66.8712633266184,6.00000000021277));
#7236=CARTESIAN_POINT('Ctrl Pts',(2.88895877345423,-66.8761604719933,6.0000000002261));
#7237=CARTESIAN_POINT('Ctrl Pts',(2.9086162068755,-66.8811071600656,6.00000000023689));
#7238=CARTESIAN_POINT('Ctrl Pts',(2.97562818114549,-66.8979703652826,6.00000000027368));
#7239=CARTESIAN_POINT('Ctrl Pts',(3.0424597316486,-66.9154094072014,6.00000000027452));
#7240=CARTESIAN_POINT('Ctrl Pts',(3.1090773696706,-66.9334077173886,6.0000000002174));
#7241=CARTESIAN_POINT('Ctrl Pts',(3.33115392136444,-66.9934068824954,6.00000000002699));
#7242=CARTESIAN_POINT('Ctrl Pts',(3.55100718513146,-67.0597320616738,6.00000000008105));
#7243=CARTESIAN_POINT('Ctrl Pts',(3.76826014113968,-67.1320917176049,6.00000000079042));
#7244=CARTESIAN_POINT('Ctrl Pts',(3.79535456432316,-67.1411159590939,6.00000000087888));
#7245=CARTESIAN_POINT('Ctrl Pts',(3.82240852080627,-67.150234120291,6.00000000097954));
#7246=CARTESIAN_POINT('Ctrl Pts',(3.84942125786838,-67.1594456880511,6.00000000109367));
#7247=CARTESIAN_POINT('Ctrl Pts',(4.06549218187766,-67.2331276682562,6.00000000200657));
#7248=CARTESIAN_POINT('Ctrl Pts',(4.27892719470564,-67.3127819172318,6.00000000402309));
#7249=CARTESIAN_POINT('Ctrl Pts',(4.49003997396306,-67.3985522392496,6.00000000629976));
#7250=CARTESIAN_POINT('Ctrl Pts',(4.52450930322692,-67.4125563439803,6.00000000667148));
#7251=CARTESIAN_POINT('Ctrl Pts',(4.55891668939615,-67.4267236013019,6.00000000704364));
#7252=CARTESIAN_POINT('Ctrl Pts',(4.59326345679802,-67.4410547629658,6.0000000074056));
#7253=CARTESIAN_POINT('Ctrl Pts',(4.91663840853981,-67.5759827070503,6.00000001081344));
#7254=CARTESIAN_POINT('Ctrl Pts',(5.23400689054315,-67.7250589551412,6.00000000260231));
#7255=CARTESIAN_POINT('Ctrl Pts',(5.54574356918105,-67.888655616953,6.00000000079463));
#7256=CARTESIAN_POINT('Ctrl Pts',(5.57540428853847,-67.9042213010907,6.00000000062264));
#7257=CARTESIAN_POINT('Ctrl Pts',(5.60501398554727,-67.9199184303487,6.00000000048578));
#7258=CARTESIAN_POINT('Ctrl Pts',(5.63457295923163,-67.935747320328,6.00000000037912));
#7259=CARTESIAN_POINT('Ctrl Pts',(5.75729333486438,-68.0014643288026,5.9999999999363));
#7260=CARTESIAN_POINT('Ctrl Pts',(5.87913955282878,-68.0694525055383,6.));
#7261=CARTESIAN_POINT('Ctrl Pts',(5.9999885243854,-68.1396985954798,6.));
#7262=CARTESIAN_POINT('',(6.,-16.9705627484771,6.));
#7263=CARTESIAN_POINT('',(6.,-68.1396788547224,6.));
#7264=CARTESIAN_POINT('',(8.,-14.8323969741913,6.));
#7265=CARTESIAN_POINT('Ctrl Pts',(6.,-16.9705627484771,6.));
#7266=CARTESIAN_POINT('Ctrl Pts',(6.,-16.7029092618308,6.));
#7267=CARTESIAN_POINT('Ctrl Pts',(6.06020384677459,-16.3874179356908,6.));
#7268=CARTESIAN_POINT('Ctrl Pts',(6.25585405294364,-15.8960743911704,6.));
#7269=CARTESIAN_POINT('Ctrl Pts',(6.42385919064368,-15.6314481148128,6.));
#7270=CARTESIAN_POINT('Ctrl Pts',(6.7778910457933,-15.2614647616422,6.));
#7271=CARTESIAN_POINT('Ctrl Pts',(7.02372732242562,-15.0877073947429,6.));
#7272=CARTESIAN_POINT('Ctrl Pts',(7.47536381734142,-14.8921163084765,6.));
#7273=CARTESIAN_POINT('Ctrl Pts',(7.75869936772315,-14.8323969741913,6.));
#7274=CARTESIAN_POINT('Ctrl Pts',(8.,-14.8323969741913,6.));
#7275=CARTESIAN_POINT('',(-8.,-14.8323969741913,6.));
#7276=CARTESIAN_POINT('',(8.,-14.8323969741913,6.));
#7277=CARTESIAN_POINT('Ctrl Pts',(-8.,-14.8323969741913,6.));
#7278=CARTESIAN_POINT('Ctrl Pts',(-7.75869936772315,-14.8323969741913,6.));
#7279=CARTESIAN_POINT('Ctrl Pts',(-7.47536381734142,-14.8921163084765,6.));
#7280=CARTESIAN_POINT('Ctrl Pts',(-7.02372732242562,-15.0877073947429,6.));
#7281=CARTESIAN_POINT('Ctrl Pts',(-6.7778910457933,-15.2614647616422,6.));
#7282=CARTESIAN_POINT('Ctrl Pts',(-6.42385919064368,-15.6314481148128,6.));
#7283=CARTESIAN_POINT('Ctrl Pts',(-6.25585405294364,-15.8960743911704,6.));
#7284=CARTESIAN_POINT('Ctrl Pts',(-6.06020384677459,-16.3874179356908,6.));
#7285=CARTESIAN_POINT('Ctrl Pts',(-6.,-16.7029092618308,6.));
#7286=CARTESIAN_POINT('Ctrl Pts',(-6.,-16.9705627484771,6.));
#7287=CARTESIAN_POINT('Origin',(0.,0.,-6.));
#7288=CARTESIAN_POINT('',(6.,-68.1396788547224,-6.));
#7289=CARTESIAN_POINT('',(6.,-16.9705627484771,-6.));
#7290=CARTESIAN_POINT('',(6.,-68.1396788547224,-6.));
#7291=CARTESIAN_POINT('',(-5.99998487131667,-68.1397397005649,-6.));
#7292=CARTESIAN_POINT('Ctrl Pts',(6.,-68.1396788547224,-6.00000000013144));
#7293=CARTESIAN_POINT('Ctrl Pts',(5.88431855295697,-68.0724390389171,-6.00000000006489));
#7294=CARTESIAN_POINT('Ctrl Pts',(5.7676591844522,-68.0072232568843,-6.00000000003826));
#7295=CARTESIAN_POINT('Ctrl Pts',(5.65004937877417,-67.9440161339786,-6.00000000002279));
#7296=CARTESIAN_POINT('Ctrl Pts',(5.3937853188605,-67.8062919549623,-5.9999999999891));
#7297=CARTESIAN_POINT('Ctrl Pts',(5.13300599736668,-67.678106939822,-6.00000000000005));
#7298=CARTESIAN_POINT('Ctrl Pts',(4.86746106690753,-67.5594828278984,-6.00000000000001));
#7299=CARTESIAN_POINT('Ctrl Pts',(4.83528148125953,-67.5451075778683,-6.));
#7300=CARTESIAN_POINT('Ctrl Pts',(4.80303195584665,-67.5308726891517,-6.));
#7301=CARTESIAN_POINT('Ctrl Pts',(4.77071208279603,-67.5167781638959,-6.));
#7302=CARTESIAN_POINT('Ctrl Pts',(4.70926493087086,-67.4899813867754,-6.));
#7303=CARTESIAN_POINT('Ctrl Pts',(4.64756353476018,-67.4636919913991,-6.));
#7304=CARTESIAN_POINT('Ctrl Pts',(4.58565379486899,-67.4379245489476,-6.));
#7305=CARTESIAN_POINT('Ctrl Pts',(4.37220621964574,-67.3490855694811,-6.));
#7306=CARTESIAN_POINT('Ctrl Pts',(4.15587960441363,-67.2662786732953,-5.99999999998255));
#7307=CARTESIAN_POINT('Ctrl Pts',(3.93822708568028,-67.19008413154,-6.00000000001744));
#7308=CARTESIAN_POINT('Ctrl Pts',(3.90982152367156,-67.1801400757894,-6.000000000022));
#7309=CARTESIAN_POINT('Ctrl Pts',(3.88139333967036,-67.1703087065859,-6.00000000002801));
#7310=CARTESIAN_POINT('Ctrl Pts',(3.8529459577009,-67.1605913714033,-6.00000000003642));
#7311=CARTESIAN_POINT('Ctrl Pts',(3.85095639975222,-67.1599117587249,-6.00000000003701));
#7312=CARTESIAN_POINT('Ctrl Pts',(3.84896674789828,-67.1592327038326,-6.00000000003761));
#7313=CARTESIAN_POINT('Ctrl Pts',(3.84697700185354,-67.1585542065258,-6.00000000003822));
#7314=CARTESIAN_POINT('Ctrl Pts',(3.59854362018346,-67.0738391843207,-6.0000000001147));
#7315=CARTESIAN_POINT('Ctrl Pts',(3.34867090555795,-66.9978150100768,-6.00000000037726));
#7316=CARTESIAN_POINT('Ctrl Pts',(3.0970148955739,-66.9301251679342,-6.0000000001887));
#7317=CARTESIAN_POINT('Ctrl Pts',(3.03668686585481,-66.9138982762787,-6.00000000014349));
#7318=CARTESIAN_POINT('Ctrl Pts',(2.97625761887668,-66.8981533988812,-6.00000000011618));
#7319=CARTESIAN_POINT('Ctrl Pts',(2.91572390730768,-66.8828865048943,-6.0000000000974));
#7320=CARTESIAN_POINT('Ctrl Pts',(2.60069430807978,-66.8034345207106,-5.99999999999966));
#7321=CARTESIAN_POINT('Ctrl Pts',(2.28283573118856,-66.7369285380892,-6.00000000005431));
#7322=CARTESIAN_POINT('Ctrl Pts',(1.96249266468246,-66.6834229474773,-6.00000000017064));
#7323=CARTESIAN_POINT('Ctrl Pts',(1.83084434322121,-66.661434267436,-6.00000000021845));
#7324=CARTESIAN_POINT('Ctrl Pts',(1.69877637473924,-66.6416411401385,-6.00000000028158));
#7325=CARTESIAN_POINT('Ctrl Pts',(1.56623212057526,-66.6240628471819,-6.00000000033809));
#7326=CARTESIAN_POINT('Ctrl Pts',(1.37616567894938,-66.5988558428255,-6.00000000041912));
#7327=CARTESIAN_POINT('Ctrl Pts',(1.18527965468047,-66.5781972427926,-6.00000000005687));
#7328=CARTESIAN_POINT('Ctrl Pts',(0.993258429335491,-66.5621547406462,-6.00000000001332));
#7329=CARTESIAN_POINT('Ctrl Pts',(0.924100321934209,-66.5563768945543,-5.99999999999763));
#7330=CARTESIAN_POINT('Ctrl Pts',(0.854794973938034,-66.5511980874682,-6.));
#7331=CARTESIAN_POINT('Ctrl Pts',(0.78537729386776,-66.54662282585,-6.));
#7332=CARTESIAN_POINT('Ctrl Pts',(0.58761689227051,-66.5335886020889,-6.));
#7333=CARTESIAN_POINT('Ctrl Pts',(0.388725531373241,-66.5254312595703,-6.00000000003796));
#7334=CARTESIAN_POINT('Ctrl Pts',(0.189932702773266,-66.5222331826198,-6.00000000006191));
#7335=CARTESIAN_POINT('Ctrl Pts',(0.129733694324287,-66.5212647318828,-6.00000000006917));
#7336=CARTESIAN_POINT('Ctrl Pts',(0.0695437634146782,-66.5207506940299,
-6.00000000006915));
#7337=CARTESIAN_POINT('Ctrl Pts',(0.00939704873694772,-66.5206924120396,
-6.00000000005797));
#7338=CARTESIAN_POINT('Ctrl Pts',(0.00486457424914242,-66.5206880200851,
-6.00000000005713));
#7339=CARTESIAN_POINT('Ctrl Pts',(0.000332345131820627,-66.5206862160106,
-6.00000000005623));
#7340=CARTESIAN_POINT('Ctrl Pts',(-0.00419963646448403,-66.5206869989526,
-6.00000000005528));
#7341=CARTESIAN_POINT('Ctrl Pts',(-0.226524783799693,-66.5207254076917,
-6.0000000000086));
#7342=CARTESIAN_POINT('Ctrl Pts',(-0.448114520868727,-66.527009152027,-6.00000000000579));
#7343=CARTESIAN_POINT('Ctrl Pts',(-0.669311485207584,-66.5394717362943,
-6.00000000000955));
#7344=CARTESIAN_POINT('Ctrl Pts',(-0.770539573358165,-66.5451750857167,
-6.00000000001128));
#7345=CARTESIAN_POINT('Ctrl Pts',(-0.871685333114638,-66.5521732055682,
-6.00000000001531));
#7346=CARTESIAN_POINT('Ctrl Pts',(-0.972781317612711,-66.5604633413958,
-6.00000000003085));
#7347=CARTESIAN_POINT('Ctrl Pts',(-1.17396285232126,-66.5769607547899,-6.00000000006176));
#7348=CARTESIAN_POINT('Ctrl Pts',(-1.37494768217033,-66.598572495594,-6.00000000011194));
#7349=CARTESIAN_POINT('Ctrl Pts',(-1.57561914509455,-66.6253535036886,-6.00000000048414));
#7350=CARTESIAN_POINT('Ctrl Pts',(-1.70028466153739,-66.6419909874459,-6.00000000071536));
#7351=CARTESIAN_POINT('Ctrl Pts',(-1.82485065445227,-66.660607736393,-6.00000000050103));
#7352=CARTESIAN_POINT('Ctrl Pts',(-1.94909396401198,-66.6812022207803,-6.00000000029781));
#7353=CARTESIAN_POINT('Ctrl Pts',(-2.0848966314161,-66.7037127762663,-6.00000000007568));
#7354=CARTESIAN_POINT('Ctrl Pts',(-2.22031339976462,-66.7285864979411,-6.00000000000453));
#7355=CARTESIAN_POINT('Ctrl Pts',(-2.3549030504907,-66.7557199666411,-6.00000000000221));
#7356=CARTESIAN_POINT('Ctrl Pts',(-2.51865982162473,-66.7887335690987,-5.9999999999994));
#7357=CARTESIAN_POINT('Ctrl Pts',(-2.68130102306261,-66.8250856467162,-5.99999999999308));
#7358=CARTESIAN_POINT('Ctrl Pts',(-2.8426997479817,-66.8647055953633,-6.00000000001334));
#7359=CARTESIAN_POINT('Ctrl Pts',(-2.86572548783398,-66.8703579239735,-6.00000000001623));
#7360=CARTESIAN_POINT('Ctrl Pts',(-2.88872591532923,-66.8760768464516,-6.00000000001994));
#7361=CARTESIAN_POINT('Ctrl Pts',(-2.91170063361983,-66.8818622395366,-6.00000000002491));
#7362=CARTESIAN_POINT('Ctrl Pts',(-2.98113403408278,-66.8993466547894,-6.00000000003995));
#7363=CARTESIAN_POINT('Ctrl Pts',(-3.05033266760026,-66.9174380547095,-6.00000000006545));
#7364=CARTESIAN_POINT('Ctrl Pts',(-3.11932927971148,-66.9361435770914,-6.00000000012216));
#7365=CARTESIAN_POINT('Ctrl Pts',(-3.36477153969483,-67.0026848977026,-6.00000000032391));
#7366=CARTESIAN_POINT('Ctrl Pts',(-3.60725660149244,-67.076855084671,-6.00000000029447));
#7367=CARTESIAN_POINT('Ctrl Pts',(-3.84706864433633,-67.1586014083108,-6.00000000017254));
#7368=CARTESIAN_POINT('Ctrl Pts',(-4.09941161515419,-67.2446192325872,-6.00000000004424));
#7369=CARTESIAN_POINT('Ctrl Pts',(-4.34879490495171,-67.339026044747,-5.99999999999992));
#7370=CARTESIAN_POINT('Ctrl Pts',(-4.59498688622864,-67.4417848987278,-6.00000000000334));
#7371=CARTESIAN_POINT('Ctrl Pts',(-4.648604639256,-67.4641645831738,-6.00000000000409));
#7372=CARTESIAN_POINT('Ctrl Pts',(-4.70206437699528,-67.486936418879,-6.00000000000469));
#7373=CARTESIAN_POINT('Ctrl Pts',(-4.7553715616119,-67.510102683164,-6.00000000000505));
#7374=CARTESIAN_POINT('Ctrl Pts',(-4.93643836022568,-67.5887907875931,-6.00000000000627));
#7375=CARTESIAN_POINT('Ctrl Pts',(-5.11574645123503,-67.6720258946313,-6.00000000000435));
#7376=CARTESIAN_POINT('Ctrl Pts',(-5.29342576273543,-67.7599657462627,-6.00000000000267));
#7377=CARTESIAN_POINT('Ctrl Pts',(-5.40844988249057,-67.8168953006373,-6.00000000000159));
#7378=CARTESIAN_POINT('Ctrl Pts',(-5.52279105849346,-67.8757975188366,-6.00000000000073));
#7379=CARTESIAN_POINT('Ctrl Pts',(-5.63648028596659,-67.9367260770655,-6.00000000000035));
#7380=CARTESIAN_POINT('Ctrl Pts',(-5.75848075352519,-68.0021088117081,-5.99999999999995));
#7381=CARTESIAN_POINT('Ctrl Pts',(-5.87973098327784,-68.0698251706507,-6.));
#7382=CARTESIAN_POINT('Ctrl Pts',(-5.99996974263335,-68.1397309048551,-6.));
#7383=CARTESIAN_POINT('',(-5.99999999999999,-16.9705627484771,-6.));
#7384=CARTESIAN_POINT('',(-5.99999999999999,-16.9705627484771,-6.));
#7385=CARTESIAN_POINT('',(-7.99999999999999,-14.8323969741913,-6.));
#7386=CARTESIAN_POINT('Ctrl Pts',(-6.,-16.9705627484771,-6.));
#7387=CARTESIAN_POINT('Ctrl Pts',(-6.,-16.7029092618308,-6.));
#7388=CARTESIAN_POINT('Ctrl Pts',(-6.06020384677459,-16.3874179356908,-6.));
#7389=CARTESIAN_POINT('Ctrl Pts',(-6.25585405294364,-15.8960743911704,-6.));
#7390=CARTESIAN_POINT('Ctrl Pts',(-6.42385919064368,-15.6314481148128,-6.));
#7391=CARTESIAN_POINT('Ctrl Pts',(-6.7778910457933,-15.2614647616422,-6.));
#7392=CARTESIAN_POINT('Ctrl Pts',(-7.02372732242562,-15.0877073947429,-6.));
#7393=CARTESIAN_POINT('Ctrl Pts',(-7.47536381734142,-14.8921163084765,-6.));
#7394=CARTESIAN_POINT('Ctrl Pts',(-7.75869936772315,-14.8323969741913,-6.));
#7395=CARTESIAN_POINT('Ctrl Pts',(-8.,-14.8323969741913,-6.));
#7396=CARTESIAN_POINT('',(8.,-14.8323969741913,-6.));
#7397=CARTESIAN_POINT('',(8.,-14.8323969741913,-6.));
#7398=CARTESIAN_POINT('Ctrl Pts',(8.,-14.8323969741913,-6.));
#7399=CARTESIAN_POINT('Ctrl Pts',(7.75869936772315,-14.8323969741913,-6.));
#7400=CARTESIAN_POINT('Ctrl Pts',(7.47536381734142,-14.8921163084765,-6.));
#7401=CARTESIAN_POINT('Ctrl Pts',(7.02372732242562,-15.0877073947429,-6.));
#7402=CARTESIAN_POINT('Ctrl Pts',(6.7778910457933,-15.2614647616422,-6.));
#7403=CARTESIAN_POINT('Ctrl Pts',(6.42385919064368,-15.6314481148128,-6.));
#7404=CARTESIAN_POINT('Ctrl Pts',(6.25585405294364,-15.8960743911704,-6.));
#7405=CARTESIAN_POINT('Ctrl Pts',(6.06020384677459,-16.3874179356908,-6.));
#7406=CARTESIAN_POINT('Ctrl Pts',(6.,-16.7029092618308,-6.));
#7407=CARTESIAN_POINT('Ctrl Pts',(6.,-16.9705627484771,-6.));
#7408=CARTESIAN_POINT('Origin',(6.,-81.,6.));
#7409=CARTESIAN_POINT('Origin',(6.,0.,0.));
#7410=CARTESIAN_POINT('',(5.99999997747517,-70.5266986161245,8.18443785141233));
#7411=CARTESIAN_POINT('Ctrl Pts',(6.,-68.1397047377494,6.00000000000005));
#7412=CARTESIAN_POINT('Ctrl Pts',(6.,-68.4373158828193,5.99999994125204));
#7413=CARTESIAN_POINT('Ctrl Pts',(6.,-68.7350865689403,6.04968588989578));
#7414=CARTESIAN_POINT('Ctrl Pts',(6.,-69.3065983612443,6.24469586989208));
#7415=CARTESIAN_POINT('Ctrl Pts',(6.00000000000086,-69.5806827235788,6.39330918939534));
#7416=CARTESIAN_POINT('Ctrl Pts',(6.00000000000086,-70.0282142371682,6.76203382605757));
#7417=CARTESIAN_POINT('Ctrl Pts',(6.,-70.2089115578842,6.97327876337078));
#7418=CARTESIAN_POINT('Ctrl Pts',(6.,-70.419255711698,7.36995744983913));
#7419=CARTESIAN_POINT('Ctrl Pts',(6.00000000004193,-70.478593909457,7.53530402271511));
#7420=CARTESIAN_POINT('Ctrl Pts',(6.00000000004193,-70.5396316268949,7.86534218943114));
#7421=CARTESIAN_POINT('Ctrl Pts',(6.,-70.5451733494511,8.02524609190228));
#7422=CARTESIAN_POINT('Ctrl Pts',(6.,-70.5267003657195,8.1844379608027));
#7423=CARTESIAN_POINT('',(6.,-70.5266968882288,-8.18443804032376));
#7424=CARTESIAN_POINT('Origin',(6.,0.,0.));
#7425=CARTESIAN_POINT('Ctrl Pts',(6.,-70.5266941883794,-8.1844377270085));
#7426=CARTESIAN_POINT('Ctrl Pts',(6.,-70.545094155265,-8.02588689619588));
#7427=CARTESIAN_POINT('Ctrl Pts',(6.00000000000071,-70.5396715184363,-7.8666208745049));
#7428=CARTESIAN_POINT('Ctrl Pts',(6.00000000000071,-70.4792696976785,-7.53789411375645));
#7429=CARTESIAN_POINT('Ctrl Pts',(5.99999999997532,-70.4204873797258,-7.3731678146394));
#7430=CARTESIAN_POINT('Ctrl Pts',(5.99999999997532,-70.2115377007883,-6.97699421954287));
#7431=CARTESIAN_POINT('Ctrl Pts',(6.0000000000039,-70.0315342165176,-6.76562661457263));
#7432=CARTESIAN_POINT('Ctrl Pts',(6.0000000000039,-69.5852755560958,-6.3962832399853));
#7433=CARTESIAN_POINT('Ctrl Pts',(6.,-69.3117412488074,-6.24719387088984));
#7434=CARTESIAN_POINT('Ctrl Pts',(6.,-68.7390122653034,-6.05035683158401));
#7435=CARTESIAN_POINT('Ctrl Pts',(6.,-68.4392574758577,-6.00000296963229));
#7436=CARTESIAN_POINT('Ctrl Pts',(6.,-68.1396788547224,-6.00000000013144));
#7437=CARTESIAN_POINT('Origin',(6.,-81.,6.));
#7438=CARTESIAN_POINT('',(6.,5.99999999999994,-16.9705627484772));
#7439=CARTESIAN_POINT('',(6.00000000000004,6.00000000137574,-68.1396788547223));
#7440=CARTESIAN_POINT('',(6.,5.99999999999994,-16.9705627484772));
#7441=CARTESIAN_POINT('',(6.,-6.00000000000006,-16.9705627484771));
#7442=CARTESIAN_POINT('Origin',(6.,0.,0.));
#7443=CARTESIAN_POINT('',(6.,-6.00000000000024,-68.1396788547224));
#7444=CARTESIAN_POINT('',(6.,-6.00000000000006,-16.9705627484771));
#7445=CARTESIAN_POINT('',(5.99999998184743,-8.18443790004951,-70.5266981504358));
#7446=CARTESIAN_POINT('Ctrl Pts',(6.,-6.00000000014129,-68.1396788547224));
#7447=CARTESIAN_POINT('Ctrl Pts',(6.,-6.00000305608312,-68.4373010930767));
#7448=CARTESIAN_POINT('Ctrl Pts',(6.,-6.04969479661867,-68.7350934660561));
#7449=CARTESIAN_POINT('Ctrl Pts',(6.,-6.24470400429899,-69.3066252131869));
#7450=CARTESIAN_POINT('Ctrl Pts',(6.00000000000098,-6.3933099872563,-69.5806863242555));
#7451=CARTESIAN_POINT('Ctrl Pts',(6.00000000000098,-6.76203851696321,-70.0282149179196));
#7452=CARTESIAN_POINT('Ctrl Pts',(6.,-6.97329170868472,-70.2089173284816));
#7453=CARTESIAN_POINT('Ctrl Pts',(6.,-7.36997476707013,-70.4192602993792));
#7454=CARTESIAN_POINT('Ctrl Pts',(6.00000000002305,-7.5353194148801,-70.4785967892622));
#7455=CARTESIAN_POINT('Ctrl Pts',(6.00000000002305,-7.86535152657698,-70.539631175309));
#7456=CARTESIAN_POINT('Ctrl Pts',(6.,-8.02525083439126,-70.5451720759936));
#7457=CARTESIAN_POINT('Ctrl Pts',(6.,-8.18443797997434,-70.5266994310349));
#7458=CARTESIAN_POINT('',(6.,-8.69499227394621E-15,-71.));
#7459=CARTESIAN_POINT('Origin',(6.,0.,0.));
#7460=CARTESIAN_POINT('',(6.,8.18443804021865,-70.526696888241));
#7461=CARTESIAN_POINT('Origin',(6.,0.,0.));
#7462=CARTESIAN_POINT('Ctrl Pts',(6.,8.18443732241168,-70.5266907030083));
#7463=CARTESIAN_POINT('Ctrl Pts',(6.,8.02588523103638,-70.5450916207373));
#7464=CARTESIAN_POINT('Ctrl Pts',(5.99999999999586,7.86661749518644,-70.5396685015587));
#7465=CARTESIAN_POINT('Ctrl Pts',(5.99999999999586,7.53788974855862,-70.4792626150954));
#7466=CARTESIAN_POINT('Ctrl Pts',(6.00000000013518,7.37316514653039,-70.4204769991494));
#7467=CARTESIAN_POINT('Ctrl Pts',(6.00000000013518,6.97700277618102,-70.2115159486837));
#7468=CARTESIAN_POINT('Ctrl Pts',(6.00000000002034,6.76564989236828,-70.031506529363));
#7469=CARTESIAN_POINT('Ctrl Pts',(6.00000000002034,6.39630460490681,-69.5852188894777));
#7470=CARTESIAN_POINT('Ctrl Pts',(6.,6.2472019641686,-69.3116452689945));
#7471=CARTESIAN_POINT('Ctrl Pts',(6.,6.0503726902255,-68.7389238969686));
#7472=CARTESIAN_POINT('Ctrl Pts',(6.,6.0000144140978,-68.4392189678418));
#7473=CARTESIAN_POINT('Ctrl Pts',(6.,6.00000000309571,-68.1396788547223));
#7474=CARTESIAN_POINT('Origin',(6.,-81.,6.));
#7475=CARTESIAN_POINT('',(6.,16.9705627484771,6.));
#7476=CARTESIAN_POINT('',(6.,68.1396788547224,6.));
#7477=CARTESIAN_POINT('',(6.,16.9705627484771,6.));
#7478=CARTESIAN_POINT('',(6.,16.9705627484771,-6.));
#7479=CARTESIAN_POINT('Origin',(6.,0.,0.));
#7480=CARTESIAN_POINT('',(6.,68.1396788547224,-6.));
#7481=CARTESIAN_POINT('',(6.,16.9705627484771,-6.));
#7482=CARTESIAN_POINT('',(5.99999996627066,70.5266997009286,-8.18443773117988));
#7483=CARTESIAN_POINT('Ctrl Pts',(6.,68.1396788547224,-6.00000000027673));
#7484=CARTESIAN_POINT('Ctrl Pts',(6.,68.4373270704393,-6.00000428105949));
#7485=CARTESIAN_POINT('Ctrl Pts',(6.,68.7351416846738,-6.04970657903531));
#7486=CARTESIAN_POINT('Ctrl Pts',(6.,69.3066578408989,-6.24472384735339));
#7487=CARTESIAN_POINT('Ctrl Pts',(6.00000000000379,69.5807112996191,-6.39331409080519));
#7488=CARTESIAN_POINT('Ctrl Pts',(6.00000000000379,70.0282207454831,-6.76201643771438));
#7489=CARTESIAN_POINT('Ctrl Pts',(6.,70.2089084902967,-6.97325603566953));
#7490=CARTESIAN_POINT('Ctrl Pts',(6.,70.4192518011347,-7.36993244016015));
#7491=CARTESIAN_POINT('Ctrl Pts',(6.00000000005203,70.4785926358654,-7.53528540527057));
#7492=CARTESIAN_POINT('Ctrl Pts',(6.00000000005203,70.5396331215713,-7.86533365840252));
#7493=CARTESIAN_POINT('Ctrl Pts',(6.,70.5451755297387,-8.02524154134083));
#7494=CARTESIAN_POINT('Ctrl Pts',(6.,70.5267025420345,-8.18443790911504));
#7495=CARTESIAN_POINT('',(6.,70.5266968882319,8.1844380402973));
#7496=CARTESIAN_POINT('Origin',(6.,0.,0.));
#7497=CARTESIAN_POINT('Ctrl Pts',(6.,70.5266929827526,8.18443758706622));
#7498=CARTESIAN_POINT('Ctrl Pts',(6.,70.5450932974979,8.0258861584249));
#7499=CARTESIAN_POINT('Ctrl Pts',(5.99999999999889,70.5396704643105,7.86661938607951));
#7500=CARTESIAN_POINT('Ctrl Pts',(5.99999999999889,70.4792671686154,7.53789242311621));
#7501=CARTESIAN_POINT('Ctrl Pts',(6.00000000003674,70.4204838116755,7.37316698642186));
#7502=CARTESIAN_POINT('Ctrl Pts',(6.00000000003674,70.2115304106972,6.97699734385621));
#7503=CARTESIAN_POINT('Ctrl Pts',(6.00000000000814,70.0315248324418,6.76563460399418));
#7504=CARTESIAN_POINT('Ctrl Pts',(6.00000000000814,69.5852562206707,6.39629025610278));
#7505=CARTESIAN_POINT('Ctrl Pts',(6.,69.3117083967071,6.24719613036894));
#7506=CARTESIAN_POINT('Ctrl Pts',(6.,68.7389797637441,6.05036104748683));
#7507=CARTESIAN_POINT('Ctrl Pts',(6.,68.4392465048021,6.00000664112192));
#7508=CARTESIAN_POINT('Ctrl Pts',(6.,68.1396788547224,6.00000000065731));
#7509=CARTESIAN_POINT('Origin',(-6.,81.,6.));
#7510=CARTESIAN_POINT('',(-5.99999290989181,-6.00000000000024,-68.1397216273217));
#7511=CARTESIAN_POINT('',(-6.,-6.00000000000006,-16.9705627484771));
#7512=CARTESIAN_POINT('',(-6.,-6.00000000000024,-68.1396788547224));
#7513=CARTESIAN_POINT('',(-6.,5.99999999999994,-16.9705627484772));
#7514=CARTESIAN_POINT('Origin',(-6.,1.17789865652746E-16,0.));
#7515=CARTESIAN_POINT('',(-6.00000000000002,6.00000000097442,-68.1396788547224));
#7516=CARTESIAN_POINT('',(-6.,5.99999999999976,-68.1396788547224));
#7517=CARTESIAN_POINT('',(-6.00000002824202,8.1844377839641,-70.5266946795513));
#7518=CARTESIAN_POINT('Ctrl Pts',(-6.,6.00000000292373,-68.1396788547223));
#7519=CARTESIAN_POINT('Ctrl Pts',(-6.,6.00001391381448,-68.4372133964188));
#7520=CARTESIAN_POINT('Ctrl Pts',(-5.99999999999999,6.04969606840112,-68.7349087606943));
#7521=CARTESIAN_POINT('Ctrl Pts',(-5.99999999999999,6.24468515704947,-69.3064384243037));
#7522=CARTESIAN_POINT('Ctrl Pts',(-6.0000000000128,6.39333208418984,-69.5805779022244));
#7523=CARTESIAN_POINT('Ctrl Pts',(-6.0000000000128,6.76209102052247,-70.0281703224301));
#7524=CARTESIAN_POINT('Ctrl Pts',(-6.00000000005601,6.97333367723825,-70.2088938300498));
#7525=CARTESIAN_POINT('Ctrl Pts',(-6.00000000005601,7.37000454340887,-70.4192521725936));
#7526=CARTESIAN_POINT('Ctrl Pts',(-5.999999999998,7.53533754904914,-70.4785892063122));
#7527=CARTESIAN_POINT('Ctrl Pts',(-5.999999999998,7.86535726226597,-70.539625540259));
#7528=CARTESIAN_POINT('Ctrl Pts',(-6.,8.025254109816,-70.5451662722122));
#7529=CARTESIAN_POINT('Ctrl Pts',(-6.,8.18443751976133,-70.5266924030008));
#7530=CARTESIAN_POINT('',(-6.,-8.69499227394621E-15,-71.));
#7531=CARTESIAN_POINT('Origin',(-6.,1.23378335349421E-30,3.53369596958238E-16));
#7532=CARTESIAN_POINT('',(-6.,-8.18443766083924,-70.526696932267));
#7533=CARTESIAN_POINT('Origin',(-6.,1.23378335349421E-30,3.53369596958238E-16));
#7534=CARTESIAN_POINT('Ctrl Pts',(-5.99999999999999,-8.18443796501575,-70.526700334414));
#7535=CARTESIAN_POINT('Ctrl Pts',(-5.99999999999999,-8.02587645834891,-70.5451002268863));
#7536=CARTESIAN_POINT('Ctrl Pts',(-6.00000000003802,-7.86660059219007,-70.5396760412271));
#7537=CARTESIAN_POINT('Ctrl Pts',(-6.00000000003802,-7.53785319168903,-70.4792688770294));
#7538=CARTESIAN_POINT('Ctrl Pts',(-5.99999999999999,-7.37311459450185,-70.4204826109743));
#7539=CARTESIAN_POINT('Ctrl Pts',(-5.99999999999999,-6.97694305312581,-70.2115379778568));
#7540=CARTESIAN_POINT('Ctrl Pts',(-6.00000000000057,-6.76558623416905,-70.0315567355748));
#7541=CARTESIAN_POINT('Ctrl Pts',(-6.00000000000057,-6.39627508448911,-69.5853337607453));
#7542=CARTESIAN_POINT('Ctrl Pts',(-5.99999999999999,-6.24720735674295,-69.3118178138716));
#7543=CARTESIAN_POINT('Ctrl Pts',(-5.99999999999999,-6.05035981119347,-68.7391217993171));
#7544=CARTESIAN_POINT('Ctrl Pts',(-5.99999999999999,-6.00000000000023,-68.4393438744497));
#7545=CARTESIAN_POINT('Ctrl Pts',(-5.99999999999999,-6.00000000000024,-68.1397278083536));
#7546=CARTESIAN_POINT('Origin',(-6.,81.,6.));
#7547=CARTESIAN_POINT('Origin',(-6.,1.17789865652746E-16,0.));
#7548=CARTESIAN_POINT('',(-6.00000002044165,-70.5266952569886,-8.18443785100741));
#7549=CARTESIAN_POINT('Ctrl Pts',(-5.99999999999999,-68.1397484962748,-6.));
#7550=CARTESIAN_POINT('Ctrl Pts',(-5.99999999999999,-68.4372667215367,-6.));
#7551=CARTESIAN_POINT('Ctrl Pts',(-5.99999999999999,-68.7349424975465,-6.04964870253574));
#7552=CARTESIAN_POINT('Ctrl Pts',(-5.99999999999999,-69.3064745088027,-6.24462699368351));
#7553=CARTESIAN_POINT('Ctrl Pts',(-6.00000000000153,-69.5806092392168,-6.39328901413462));
#7554=CARTESIAN_POINT('Ctrl Pts',(-6.00000000000153,-70.0282000466676,-6.76208375846719));
#7555=CARTESIAN_POINT('Ctrl Pts',(-6.00000000035957,-70.2089294430131,-6.9733562678496));
#7556=CARTESIAN_POINT('Ctrl Pts',(-6.00000000035957,-70.4192721255049,-7.37004589750889));
#7557=CARTESIAN_POINT('Ctrl Pts',(-5.99999999998651,-70.4786003297255,-7.53537093001657));
#7558=CARTESIAN_POINT('Ctrl Pts',(-5.99999999998651,-70.5396271011112,-7.8653738247129));
#7559=CARTESIAN_POINT('Ctrl Pts',(-5.99999999999999,-70.5451662208239,-8.0252622570676));
#7560=CARTESIAN_POINT('Ctrl Pts',(-5.99999999999999,-70.5266935751337,-8.18443765582455));
#7561=CARTESIAN_POINT('',(-5.99999998001766,-70.5266982778411,8.18443788597873));
#7562=CARTESIAN_POINT('Origin',(-6.,-3.53369596958238E-16,0.));
#7563=CARTESIAN_POINT('Ctrl Pts',(-5.99999999999999,-70.5266996874987,8.18443797574402));
#7564=CARTESIAN_POINT('Ctrl Pts',(-5.99999999999999,-70.5450992579752,8.0258803335721));
#7565=CARTESIAN_POINT('Ctrl Pts',(-6.00000000002134,-70.5396757507429,7.86660830835082));
#7566=CARTESIAN_POINT('Ctrl Pts',(-6.00000000002134,-70.4792714259724,7.53786559283121));
#7567=CARTESIAN_POINT('Ctrl Pts',(-5.99999999999999,-70.42048657203,7.37312821110373));
#7568=CARTESIAN_POINT('Ctrl Pts',(-5.99999999999999,-70.2115435781299,6.97695270225775));
#7569=CARTESIAN_POINT('Ctrl Pts',(-6.00000000000098,-70.031558716588,6.76558800338714));
#7570=CARTESIAN_POINT('Ctrl Pts',(-6.00000000000098,-69.5853412925519,6.39627546000802));
#7571=CARTESIAN_POINT('Ctrl Pts',(-5.99999999999999,-69.3118535798659,6.24721921781684));
#7572=CARTESIAN_POINT('Ctrl Pts',(-5.99999999999999,-68.739127923668,6.05037041272747));
#7573=CARTESIAN_POINT('Ctrl Pts',(-5.99999999999999,-68.4393146647117,6.00000293652382));
#7574=CARTESIAN_POINT('Ctrl Pts',(-5.99999999999999,-68.1396788547224,6.00000000012849));
#7575=CARTESIAN_POINT('Origin',(-6.,81.,6.));
#7576=CARTESIAN_POINT('',(-5.99999999999999,6.00000000000006,16.9705627484771));
#7577=CARTESIAN_POINT('',(-5.99999999999999,6.00000000000024,68.1396788547224));
#7578=CARTESIAN_POINT('',(-5.99999999999999,6.00000000000006,16.9705627484771));
#7579=CARTESIAN_POINT('',(-5.99999999999999,-5.99999999999994,16.9705627484772));
#7580=CARTESIAN_POINT('Origin',(-6.,1.17789865652746E-16,0.));
#7581=CARTESIAN_POINT('',(-5.99999800383455,-5.99999999999981,68.1396904583549));
#7582=CARTESIAN_POINT('',(-5.99999999999999,-5.99999999999994,16.9705627484772));
#7583=CARTESIAN_POINT('',(-5.99999997386433,-8.18443780213022,70.5266990636957));
#7584=CARTESIAN_POINT('Ctrl Pts',(-5.99999999999999,-5.99999999999991,68.1396917580846));
#7585=CARTESIAN_POINT('Ctrl Pts',(-5.99999999999999,-5.99999990221501,68.4373180189636));
#7586=CARTESIAN_POINT('Ctrl Pts',(-6.,-6.04969214680078,68.73510741349));
#7587=CARTESIAN_POINT('Ctrl Pts',(-6.,-6.24470617061769,69.3066184436945));
#7588=CARTESIAN_POINT('Ctrl Pts',(-6.00000000000163,-6.39331179161704,69.5806934109985));
#7589=CARTESIAN_POINT('Ctrl Pts',(-6.00000000000163,-6.76202707922547,70.0282163865669));
#7590=CARTESIAN_POINT('Ctrl Pts',(-5.99999999999999,-6.97326897652041,70.2089096425642));
#7591=CARTESIAN_POINT('Ctrl Pts',(-5.99999999999999,-7.36994644175672,70.4192537935309));
#7592=CARTESIAN_POINT('Ctrl Pts',(-6.00000000004821,-7.53529576254731,70.4785932103609));
#7593=CARTESIAN_POINT('Ctrl Pts',(-6.00000000004821,-7.86533835046211,70.5396322309098));
#7594=CARTESIAN_POINT('Ctrl Pts',(-6.,-8.02524406228223,70.5451742661205));
#7595=CARTESIAN_POINT('Ctrl Pts',(-6.,-8.18443793975999,70.5267012613836));
#7596=CARTESIAN_POINT('',(-6.00000002044842,8.18443786845297,70.5266954072364));
#7597=CARTESIAN_POINT('Origin',(-6.,1.23378335349421E-30,3.53369596958238E-16));
#7598=CARTESIAN_POINT('Ctrl Pts',(-6.,8.1844376908963,70.5266938772528));
#7599=CARTESIAN_POINT('Ctrl Pts',(-6.,8.02588660831281,70.545093945321));
#7600=CARTESIAN_POINT('Ctrl Pts',(-6.00000000000021,7.86662029545443,70.5396712396839));
#7601=CARTESIAN_POINT('Ctrl Pts',(-6.00000000000021,7.53789345525426,70.4792689721846));
#7602=CARTESIAN_POINT('Ctrl Pts',(-5.99999999999207,7.37316744126058,70.4204863862969));
#7603=CARTESIAN_POINT('Ctrl Pts',(-5.99999999999207,6.97699496825595,70.2115357634242));
#7604=CARTESIAN_POINT('Ctrl Pts',(-6.00000000000484,6.7656286627794,70.0315317575654));
#7605=CARTESIAN_POINT('Ctrl Pts',(-6.00000000000484,6.39628501585991,69.5852704695977));
#7606=CARTESIAN_POINT('Ctrl Pts',(-5.99999999999999,6.24719439633593,69.3117325652093));
#7607=CARTESIAN_POINT('Ctrl Pts',(-5.99999999999999,6.05035712202607,68.7390013313318));
#7608=CARTESIAN_POINT('Ctrl Pts',(-5.99999999999999,6.0000039352936,68.4392570047814));
#7609=CARTESIAN_POINT('Ctrl Pts',(-5.99999999999999,6.00000000023106,68.1396788547224));
#7610=CARTESIAN_POINT('Origin',(0.,0.,6.));
#7611=CARTESIAN_POINT('',(-5.99999659392154,68.1396991687892,6.00000000000001));
#7612=CARTESIAN_POINT('Ctrl Pts',(6.00000000000002,68.1396788547224,6.00000000065731));
#7613=CARTESIAN_POINT('Ctrl Pts',(5.88458780655166,68.0725952090573,6.0000000003255));
#7614=CARTESIAN_POINT('Ctrl Pts',(5.7681428376056,68.0075008237318,6.00000000024891));
#7615=CARTESIAN_POINT('Ctrl Pts',(5.65067183885126,67.9443722158119,6.00000000020361));
#7616=CARTESIAN_POINT('Ctrl Pts',(5.38642690984633,67.8023676811193,6.00000000010169));
#7617=CARTESIAN_POINT('Ctrl Pts',(5.11699288348237,67.6703133164605,6.00000000024462));
#7618=CARTESIAN_POINT('Ctrl Pts',(4.84313854685597,67.5486842141237,6.00000000017594));
#7619=CARTESIAN_POINT('Ctrl Pts',(4.81851114481416,67.5377462503867,6.00000000016977));
#7620=CARTESIAN_POINT('Ctrl Pts',(4.79384797350979,67.526892570235,6.00000000016207));
#7621=CARTESIAN_POINT('Ctrl Pts',(4.76914957931904,67.5161235029138,6.00000000015292));
#7622=CARTESIAN_POINT('Ctrl Pts',(4.70749169934415,67.4892392506337,6.00000000013006));
#7623=CARTESIAN_POINT('Ctrl Pts',(4.64561433330076,67.4628823302612,6.00000000009686));
#7624=CARTESIAN_POINT('Ctrl Pts',(4.58355358413935,67.4370609019436,6.00000000006413));
#7625=CARTESIAN_POINT('Ctrl Pts',(4.3984410260912,67.3600416794412,5.99999999996652));
#7626=CARTESIAN_POINT('Ctrl Pts',(4.21149574112703,67.2877208487954,5.9999999999379));
#7627=CARTESIAN_POINT('Ctrl Pts',(4.02339026402838,67.220280599234,6.00000000006967));
#7628=CARTESIAN_POINT('Ctrl Pts',(3.96640526002753,67.1998501314435,6.00000000010959));
#7629=CARTESIAN_POINT('Ctrl Pts',(3.90931362085271,67.1798679001431,6.0000000001777));
#7630=CARTESIAN_POINT('Ctrl Pts',(3.85213373160562,67.1603398560627,6.00000000033226));
#7631=CARTESIAN_POINT('Ctrl Pts',(3.85016142643025,67.1596662754924,6.0000000003376));
#7632=CARTESIAN_POINT('Ctrl Pts',(3.84818901625124,67.1589932353419,6.00000000034303));
#7633=CARTESIAN_POINT('Ctrl Pts',(3.84621650069232,67.1583207354738,6.00000000034858));
#7634=CARTESIAN_POINT('Ctrl Pts',(3.5982890765688,67.0737935644395,6.00000000104606));
#7635=CARTESIAN_POINT('Ctrl Pts',(3.3486968786768,66.9978617665185,6.00000001076173));
#7636=CARTESIAN_POINT('Ctrl Pts',(3.09725398859764,66.9301813536615,6.00000001025565));
#7637=CARTESIAN_POINT('Ctrl Pts',(2.76617148958911,66.8410644960898,6.00000000958927));
#7638=CARTESIAN_POINT('Ctrl Pts',(2.43192850502006,66.7664323064067,6.00000000286088));
#7639=CARTESIAN_POINT('Ctrl Pts',(2.09397569559093,66.706165144386,6.00000000174086));
#7640=CARTESIAN_POINT('Ctrl Pts',(2.05038959937716,66.6983924310098,6.00000000159641));
#7641=CARTESIAN_POINT('Ctrl Pts',(2.00674184718961,66.6908587070349,6.00000000150129));
#7642=CARTESIAN_POINT('Ctrl Pts',(1.96303130641295,66.6835637569233,6.00000000145524));
#7643=CARTESIAN_POINT('Ctrl Pts',(1.83087276517514,66.6615075217903,6.00000000131602));
#7644=CARTESIAN_POINT('Ctrl Pts',(1.69814016267927,66.6416339787774,6.00000000143221));
#7645=CARTESIAN_POINT('Ctrl Pts',(1.56485129042034,66.6239976603168,6.00000000294475));
#7646=CARTESIAN_POINT('Ctrl Pts',(1.37465928224473,66.5988321174775,6.00000000510302));
#7647=CARTESIAN_POINT('Ctrl Pts',(1.18358970013618,66.5781827823755,6.00000000620398));
#7648=CARTESIAN_POINT('Ctrl Pts',(0.991617758843105,66.5621619254138,6.0000000057091));
#7649=CARTESIAN_POINT('Ctrl Pts',(0.740815052328747,66.5412313964019,6.00000000506256));
#7650=CARTESIAN_POINT('Ctrl Pts',(0.488472212738995,66.5281989642491,6.00000000262167));
#7651=CARTESIAN_POINT('Ctrl Pts',(0.236328250644454,66.523133255531,6.00000000145786));
#7652=CARTESIAN_POINT('Ctrl Pts',(0.159870466408439,66.5215971772488,6.00000000110496));
#7653=CARTESIAN_POINT('Ctrl Pts',(0.0834309792026766,66.5207939914652,6.00000000083788));
#7654=CARTESIAN_POINT('Ctrl Pts',(0.00705844255551847,66.5207265533995,
6.00000000064985));
#7655=CARTESIAN_POINT('Ctrl Pts',(0.00181350859966491,66.5207219220462,
6.00000000063694));
#7656=CARTESIAN_POINT('Ctrl Pts',(-0.00343110952298811,66.5207207609042,
6.00000000062438));
#7657=CARTESIAN_POINT('Ctrl Pts',(-0.00867542023187034,66.5207230706085,
6.00000000061218));
#7658=CARTESIAN_POINT('Ctrl Pts',(-0.331628834827677,66.5208653060567,5.99999999986073));
#7659=CARTESIAN_POINT('Ctrl Pts',(-0.653114357046965,66.5341608814007,6.00000000001333));
#7660=CARTESIAN_POINT('Ctrl Pts',(-0.974743165742799,66.560621565599,6.00000000001792));
#7661=CARTESIAN_POINT('Ctrl Pts',(-1.17715728160842,66.5772743524525,6.00000000002081));
#7662=CARTESIAN_POINT('Ctrl Pts',(-1.37962806781815,66.5991418583686,6.00000000003358));
#7663=CARTESIAN_POINT('Ctrl Pts',(-1.58132881881509,66.6261417714914,6.00000000014743));
#7664=CARTESIAN_POINT('Ctrl Pts',(-1.70522987986189,66.6427273214586,6.00000000021737));
#7665=CARTESIAN_POINT('Ctrl Pts',(-1.82905078205798,66.6612792878494,6.00000000033522));
#7666=CARTESIAN_POINT('Ctrl Pts',(-1.95241072789507,66.6817574578459,6.00000000038641));
#7667=CARTESIAN_POINT('Ctrl Pts',(-2.08900850840277,66.7044331533596,6.00000000044308));
#7668=CARTESIAN_POINT('Ctrl Pts',(-2.2250405745722,66.7294710847112,6.00000000035428));
#7669=CARTESIAN_POINT('Ctrl Pts',(-2.3601828255349,66.7567627898884,6.00000000017272));
#7670=CARTESIAN_POINT('Ctrl Pts',(-2.52887378089362,66.7908295882947,5.99999999994608));
#7671=CARTESIAN_POINT('Ctrl Pts',(-2.69612953033057,66.8284193088917,6.00000000000241));
#7672=CARTESIAN_POINT('Ctrl Pts',(-2.86209194811488,66.8694715270266,6.00000000000268));
#7673=CARTESIAN_POINT('Ctrl Pts',(-2.87883967552237,66.8736142201012,6.00000000000271));
#7674=CARTESIAN_POINT('Ctrl Pts',(-2.89557422162999,66.8777922154813,6.00000000000284));
#7675=CARTESIAN_POINT('Ctrl Pts',(-2.91229572454255,66.8820054793396,6.00000000000307));
#7676=CARTESIAN_POINT('Ctrl Pts',(-2.9825032438285,66.8996954444783,6.00000000000407));
#7677=CARTESIAN_POINT('Ctrl Pts',(-3.0524808714627,66.9180070193092,6.00000000000678));
#7678=CARTESIAN_POINT('Ctrl Pts',(-3.12225265070286,66.9369440322735,6.00000000001525));
#7679=CARTESIAN_POINT('Ctrl Pts',(-3.36632242546284,67.0031878996244,6.0000000000449));
#7680=CARTESIAN_POINT('Ctrl Pts',(-3.60783909617146,67.0770801580024,6.00000000017843));
#7681=CARTESIAN_POINT('Ctrl Pts',(-3.84666540906819,67.1584730795796,6.00000000030431));
#7682=CARTESIAN_POINT('Ctrl Pts',(-4.07435177258606,67.2360694637687,6.00000000042432));
#7683=CARTESIAN_POINT('Ctrl Pts',(-4.29959331275655,67.3204828589082,6.00000000045655));
#7684=CARTESIAN_POINT('Ctrl Pts',(-4.52242840730631,67.4117842364616,6.00000000027812));
#7685=CARTESIAN_POINT('Ctrl Pts',(-4.54672655587405,67.4217398246543,6.00000000025867));
#7686=CARTESIAN_POINT('Ctrl Pts',(-4.57099610644136,67.4317772614459,6.00000000023763));
#7687=CARTESIAN_POINT('Ctrl Pts',(-4.59523711898079,67.4418966025886,6.0000000002158));
#7688=CARTESIAN_POINT('Ctrl Pts',(-4.64891007134559,67.464302222578,6.00000000016746));
#7689=CARTESIAN_POINT('Ctrl Pts',(-4.70242464530625,67.4871028602993,6.00000000013265));
#7690=CARTESIAN_POINT('Ctrl Pts',(-4.75579883589029,67.5103059640663,6.0000000001061));
#7691=CARTESIAN_POINT('Ctrl Pts',(-4.90528832196,67.5752928054479,6.00000000003174));
#7692=CARTESIAN_POINT('Ctrl Pts',(-5.05367780331171,67.6434327643659,6.0000000000171));
#7693=CARTESIAN_POINT('Ctrl Pts',(-5.20095707175058,67.7147496307297,6.00000000000847));
#7694=CARTESIAN_POINT('Ctrl Pts',(-5.34823634018945,67.7860664970935,5.99999999999985));
#7695=CARTESIAN_POINT('Ctrl Pts',(-5.49440633438804,67.8605605910626,6.00000000000048));
#7696=CARTESIAN_POINT('Ctrl Pts',(-5.63943167744069,67.9383073892477,6.00000000000019));
#7697=CARTESIAN_POINT('Ctrl Pts',(-5.76042394103096,68.0031702670131,5.99999999999995));
#7698=CARTESIAN_POINT('Ctrl Pts',(-5.88061928742128,68.0702983394636,6.));
#7699=CARTESIAN_POINT('Ctrl Pts',(-5.99998978176463,68.1396964325479,6.));
#7700=CARTESIAN_POINT('',(-6.,16.9705627484771,6.));
#7701=CARTESIAN_POINT('',(-6.,68.1396788547224,6.));
#7702=CARTESIAN_POINT('',(-8.,14.8323969741913,6.));
#7703=CARTESIAN_POINT('Ctrl Pts',(-6.,16.9705627484771,6.));
#7704=CARTESIAN_POINT('Ctrl Pts',(-6.,16.7029092618308,6.));
#7705=CARTESIAN_POINT('Ctrl Pts',(-6.06020384677459,16.3874179356908,6.));
#7706=CARTESIAN_POINT('Ctrl Pts',(-6.25585405294364,15.8960743911704,6.));
#7707=CARTESIAN_POINT('Ctrl Pts',(-6.42385919064368,15.6314481148128,6.));
#7708=CARTESIAN_POINT('Ctrl Pts',(-6.7778910457933,15.2614647616422,6.));
#7709=CARTESIAN_POINT('Ctrl Pts',(-7.02372732242562,15.0877073947429,6.));
#7710=CARTESIAN_POINT('Ctrl Pts',(-7.47536381734142,14.8921163084765,6.));
#7711=CARTESIAN_POINT('Ctrl Pts',(-7.75869936772315,14.8323969741913,6.));
#7712=CARTESIAN_POINT('Ctrl Pts',(-8.,14.8323969741913,6.));
#7713=CARTESIAN_POINT('',(8.,14.8323969741913,6.));
#7714=CARTESIAN_POINT('',(8.,14.8323969741913,6.));
#7715=CARTESIAN_POINT('Ctrl Pts',(8.,14.8323969741913,6.));
#7716=CARTESIAN_POINT('Ctrl Pts',(7.75869936772315,14.8323969741913,6.));
#7717=CARTESIAN_POINT('Ctrl Pts',(7.47536381734142,14.8921163084765,6.));
#7718=CARTESIAN_POINT('Ctrl Pts',(7.02372732242562,15.0877073947429,6.));
#7719=CARTESIAN_POINT('Ctrl Pts',(6.7778910457933,15.2614647616422,6.));
#7720=CARTESIAN_POINT('Ctrl Pts',(6.42385919064368,15.6314481148128,6.));
#7721=CARTESIAN_POINT('Ctrl Pts',(6.25585405294364,15.8960743911704,6.));
#7722=CARTESIAN_POINT('Ctrl Pts',(6.06020384677459,16.3874179356908,6.));
#7723=CARTESIAN_POINT('Ctrl Pts',(6.,16.7029092618308,6.));
#7724=CARTESIAN_POINT('Ctrl Pts',(6.,16.9705627484771,6.));
#7725=CARTESIAN_POINT('Origin',(0.,0.,-6.));
#7726=CARTESIAN_POINT('',(-6.,68.1396788547224,-6.));
#7727=CARTESIAN_POINT('',(-6.,16.9705627484771,-6.));
#7728=CARTESIAN_POINT('',(-6.,68.1396788547224,-6.));
#7729=CARTESIAN_POINT('Ctrl Pts',(-6.00000000000001,68.1396788547224,-6.00000000033548));
#7730=CARTESIAN_POINT('Ctrl Pts',(-5.88135123476548,68.0707064539889,-6.00000000021859));
#7731=CARTESIAN_POINT('Ctrl Pts',(-5.76179150219477,68.0039433666279,-6.0000000001483));
#7732=CARTESIAN_POINT('Ctrl Pts',(-5.64128502565881,67.9393234853503,-6.00000000010555));
#7733=CARTESIAN_POINT('Ctrl Pts',(-5.35454183345322,67.7855615335439,-6.00000000000383));
#7734=CARTESIAN_POINT('Ctrl Pts',(-5.06243931289424,67.6439341165104,-5.99999999997568));
#7735=CARTESIAN_POINT('Ctrl Pts',(-4.7653752487817,67.51447477604,-6.00000000011691));
#7736=CARTESIAN_POINT('Ctrl Pts',(-4.70765521754892,67.4893206154462,-6.00000000014435));
#7737=CARTESIAN_POINT('Ctrl Pts',(-4.64974783530638,67.4646258594542,-6.00000000018246));
#7738=CARTESIAN_POINT('Ctrl Pts',(-4.59164625233319,67.440390106457,-6.00000000024038));
#7739=CARTESIAN_POINT('Ctrl Pts',(-4.35024698211367,67.3396958949164,-6.00000000048101));
#7740=CARTESIAN_POINT('Ctrl Pts',(-4.10557127976831,67.2469034855812,-6.00000000012488));
#7741=CARTESIAN_POINT('Ctrl Pts',(-3.857028682324,67.1619865543543,-6.00000000004164));
#7742=CARTESIAN_POINT('Ctrl Pts',(-3.85632817266295,67.1617472185973,-6.0000000000414));
#7743=CARTESIAN_POINT('Ctrl Pts',(-3.85562763231577,67.161507945473,-6.00000000004117));
#7744=CARTESIAN_POINT('Ctrl Pts',(-3.85492706127251,67.161268734981,-6.00000000004094));
#7745=CARTESIAN_POINT('Ctrl Pts',(-3.60706325630569,67.0766354585685,-5.9999999999591));
#7746=CARTESIAN_POINT('Ctrl Pts',(-3.35536071028375,66.9998438175543,-6.));
#7747=CARTESIAN_POINT('Ctrl Pts',(-3.10247303323778,66.9316279187809,-6.));
#7748=CARTESIAN_POINT('Ctrl Pts',(-3.03891432167408,66.9144830950993,-6.));
#7749=CARTESIAN_POINT('Ctrl Pts',(-2.97524844790974,66.8978716712467,-5.99999999999992));
#7750=CARTESIAN_POINT('Ctrl Pts',(-2.91151863585045,66.8818072455702,-6.00000000000031));
#7751=CARTESIAN_POINT('Ctrl Pts',(-2.63102181288571,66.8111021827525,-6.00000000000201));
#7752=CARTESIAN_POINT('Ctrl Pts',(-2.34928633703758,66.7509976829606,-6.0000000000383));
#7753=CARTESIAN_POINT('Ctrl Pts',(-2.06637325397113,66.7012185486804,-6.00000000006218));
#7754=CARTESIAN_POINT('Ctrl Pts',(-2.02907999731538,66.694656724071,-6.00000000006533));
#7755=CARTESIAN_POINT('Ctrl Pts',(-1.99176628159546,66.6882742410331,-6.00000000006784));
#7756=CARTESIAN_POINT('Ctrl Pts',(-1.95443224984977,66.6820704027054,-6.00000000006935));
#7757=CARTESIAN_POINT('Ctrl Pts',(-1.82582569506263,66.6606997058783,-6.00000000007455));
#7758=CARTESIAN_POINT('Ctrl Pts',(-1.69697805757653,66.6414490286518,-6.00000000006504));
#7759=CARTESIAN_POINT('Ctrl Pts',(-1.56792279424157,66.6243169437229,-6.00000000004334));
#7760=CARTESIAN_POINT('Ctrl Pts',(-1.37527749253196,66.5987432818299,-6.00000000001095));
#7761=CARTESIAN_POINT('Ctrl Pts',(-1.18208097804144,66.5778870888126,-6.00000000000977));
#7762=CARTESIAN_POINT('Ctrl Pts',(-0.988407256485119,66.5617481221748,-6.00000000000759));
#7763=CARTESIAN_POINT('Ctrl Pts',(-0.665022342205425,66.5348002311508,-6.00000000000395));
#7764=CARTESIAN_POINT('Ctrl Pts',(-0.340306945124361,66.5210055006354,-6.00000000000648));
#7765=CARTESIAN_POINT('Ctrl Pts',(-0.0134586100326744,66.5206838218603,
-6.00000000000188));
#7766=CARTESIAN_POINT('Ctrl Pts',(-0.0124519601418355,66.5206828311319,
-6.00000000000187));
#7767=CARTESIAN_POINT('Ctrl Pts',(-0.0114452900197199,66.5206819681829,
-6.00000000000185));
#7768=CARTESIAN_POINT('Ctrl Pts',(-0.0104385997885719,66.5206812330135,
-6.00000000000184));
#7769=CARTESIAN_POINT('Ctrl Pts',(0.251373358176787,66.5204900360357,-5.99999999999816));
#7770=CARTESIAN_POINT('Ctrl Pts',(0.514448035954128,66.5289433967365,-6.));
#7771=CARTESIAN_POINT('Ctrl Pts',(0.776872929457171,66.5460551200837,-6.));
#7772=CARTESIAN_POINT('Ctrl Pts',(0.84113945443676,66.5502456943134,-6.));
#7773=CARTESIAN_POINT('Ctrl Pts',(0.905383773332602,66.5549590297467,-5.99999999999899));
#7774=CARTESIAN_POINT('Ctrl Pts',(0.96956591794925,66.5601942307276,-6.0000000000062));
#7775=CARTESIAN_POINT('Ctrl Pts',(1.16746410942001,66.5763363651527,-6.00000000002842));
#7776=CARTESIAN_POINT('Ctrl Pts',(1.36476998969738,66.597443812802,-6.00000000018961));
#7777=CARTESIAN_POINT('Ctrl Pts',(1.56118391871842,66.6233966302541,-6.00000000007553));
#7778=CARTESIAN_POINT('Ctrl Pts',(1.68948047047876,66.6403488749558,-6.00000000000101));
#7779=CARTESIAN_POINT('Ctrl Pts',(1.81736883731735,66.6593790563258,-6.00000000000495));
#7780=CARTESIAN_POINT('Ctrl Pts',(1.94492176430178,66.6804804617521,-6.00000000000425));
#7781=CARTESIAN_POINT('Ctrl Pts',(2.07597587522071,66.7021610769498,-6.00000000000353));
#7782=CARTESIAN_POINT('Ctrl Pts',(2.20667590863535,66.7260281326416,-5.9999999999992));
#7783=CARTESIAN_POINT('Ctrl Pts',(2.33707867056231,66.7521088426973,-6.00000000006009));
#7784=CARTESIAN_POINT('Ctrl Pts',(2.52789038140951,66.7902714155777,-6.00000000014919));
#7785=CARTESIAN_POINT('Ctrl Pts',(2.71803095889827,66.8331402961369,-6.00000000004381));
#7786=CARTESIAN_POINT('Ctrl Pts',(2.90717461949266,66.8807206424077,-6.00000000001451));
#7787=CARTESIAN_POINT('Ctrl Pts',(2.97310322799981,66.897305422527,-6.0000000000043));
#7788=CARTESIAN_POINT('Ctrl Pts',(3.03891073048377,66.9144622409335,-6.0000000000018));
#7789=CARTESIAN_POINT('Ctrl Pts',(3.10455475004544,66.932177232458,-6.00000000000118));
#7790=CARTESIAN_POINT('Ctrl Pts',(3.30454500276501,66.9861475050824,-5.99999999999932));
#7791=CARTESIAN_POINT('Ctrl Pts',(3.50317683929644,67.045322334494,-5.99999999998744));
#7792=CARTESIAN_POINT('Ctrl Pts',(3.69973730005121,67.1094558520618,-6.00000000001292));
#7793=CARTESIAN_POINT('Ctrl Pts',(3.7500829322271,67.1258825661284,-6.00000000001944));
#7794=CARTESIAN_POINT('Ctrl Pts',(3.80029253777679,67.1426348178705,-6.00000000002988));
#7795=CARTESIAN_POINT('Ctrl Pts',(3.85035380604943,67.1597089272837,-6.00000000005043));
#7796=CARTESIAN_POINT('Ctrl Pts',(3.85304807262321,67.1606278453187,-6.00000000005154));
#7797=CARTESIAN_POINT('Ctrl Pts',(3.85574190949298,67.1615476956639,-6.00000000005268));
#7798=CARTESIAN_POINT('Ctrl Pts',(3.85843531784378,67.1624684786439,-6.00000000005384));
#7799=CARTESIAN_POINT('Ctrl Pts',(4.10656203133196,67.247294403611,-6.00000000016149));
#7800=CARTESIAN_POINT('Ctrl Pts',(4.35103204358516,67.3400159519093,-6.00000000044336));
#7801=CARTESIAN_POINT('Ctrl Pts',(4.5922509791071,67.4406456432544,-6.00000000022157));
#7802=CARTESIAN_POINT('Ctrl Pts',(4.64834046407308,67.4640445839206,-6.00000000016999));
#7803=CARTESIAN_POINT('Ctrl Pts',(4.70424963404129,67.4878714386743,-6.00000000013519));
#7804=CARTESIAN_POINT('Ctrl Pts',(4.75998502568673,67.5121269723368,-6.00000000010976));
#7805=CARTESIAN_POINT('Ctrl Pts',(5.05700416524726,67.6413869905284,-5.99999999997425));
#7806=CARTESIAN_POINT('Ctrl Pts',(5.34908932208966,67.7828195726981,-6.00000000000132));
#7807=CARTESIAN_POINT('Ctrl Pts',(5.63593680564189,67.9364541673593,-6.00000000008223));
#7808=CARTESIAN_POINT('Ctrl Pts',(5.75823770305734,68.0019581368152,-6.00000000011673));
#7809=CARTESIAN_POINT('Ctrl Pts',(5.879586265764,68.0696804496391,-6.00000000017492));
#7810=CARTESIAN_POINT('Ctrl Pts',(5.99999999999993,68.1396788547225,-6.00000000027673));
#7811=CARTESIAN_POINT('',(8.,14.8323969741913,-6.));
#7812=CARTESIAN_POINT('Ctrl Pts',(6.,16.9705627484771,-6.));
#7813=CARTESIAN_POINT('Ctrl Pts',(6.,16.7029092618308,-6.));
#7814=CARTESIAN_POINT('Ctrl Pts',(6.06020384677459,16.3874179356908,-6.));
#7815=CARTESIAN_POINT('Ctrl Pts',(6.25585405294364,15.8960743911704,-6.));
#7816=CARTESIAN_POINT('Ctrl Pts',(6.42385919064368,15.6314481148128,-6.));
#7817=CARTESIAN_POINT('Ctrl Pts',(6.7778910457933,15.2614647616422,-6.));
#7818=CARTESIAN_POINT('Ctrl Pts',(7.02372732242562,15.0877073947429,-6.));
#7819=CARTESIAN_POINT('Ctrl Pts',(7.47536381734142,14.8921163084765,-6.));
#7820=CARTESIAN_POINT('Ctrl Pts',(7.75869936772315,14.8323969741913,-6.));
#7821=CARTESIAN_POINT('Ctrl Pts',(8.,14.8323969741913,-6.));
#7822=CARTESIAN_POINT('',(-8.,14.8323969741913,-6.));
#7823=CARTESIAN_POINT('',(8.,14.8323969741913,-6.));
#7824=CARTESIAN_POINT('Ctrl Pts',(-8.,14.8323969741913,-6.));
#7825=CARTESIAN_POINT('Ctrl Pts',(-7.75869936772315,14.8323969741913,-6.));
#7826=CARTESIAN_POINT('Ctrl Pts',(-7.47536381734142,14.8921163084765,-6.));
#7827=CARTESIAN_POINT('Ctrl Pts',(-7.02372732242562,15.0877073947429,-6.));
#7828=CARTESIAN_POINT('Ctrl Pts',(-6.7778910457933,15.2614647616422,-6.));
#7829=CARTESIAN_POINT('Ctrl Pts',(-6.42385919064368,15.6314481148128,-6.));
#7830=CARTESIAN_POINT('Ctrl Pts',(-6.25585405294364,15.8960743911704,-6.));
#7831=CARTESIAN_POINT('Ctrl Pts',(-6.06020384677459,16.3874179356908,-6.));
#7832=CARTESIAN_POINT('Ctrl Pts',(-6.,16.7029092618308,-6.));
#7833=CARTESIAN_POINT('Ctrl Pts',(-6.,16.9705627484771,-6.));
#7834=CARTESIAN_POINT('Origin',(0.,6.,-2.09488880330588E-14));
#7835=CARTESIAN_POINT('Ctrl Pts',(6.00000000000008,6.00000000309571,-68.1396788547223));
#7836=CARTESIAN_POINT('Ctrl Pts',(5.88443053952251,6.00000000152898,-68.0725017211956));
#7837=CARTESIAN_POINT('Ctrl Pts',(5.76781164854468,6.00000000116511,-68.0073271284604));
#7838=CARTESIAN_POINT('Ctrl Pts',(5.65007008364704,6.00000000095536,-67.9440866077606));
#7839=CARTESIAN_POINT('Ctrl Pts',(5.47466763156413,6.0000000006429,-67.8498756771399));
#7840=CARTESIAN_POINT('Ctrl Pts',(5.29677696751753,6.000000000858,-67.7599563862543));
#7841=CARTESIAN_POINT('Ctrl Pts',(5.11705077455563,6.00000000100214,-67.6746189934296));
#7842=CARTESIAN_POINT('Ctrl Pts',(5.00046956793888,6.00000000109564,-67.6192640334147));
#7843=CARTESIAN_POINT('Ctrl Pts',(4.88311488344197,6.00000000115652,-67.565837369108));
#7844=CARTESIAN_POINT('Ctrl Pts',(4.76515531729687,6.00000000101204,-67.5144247705252));
#7845=CARTESIAN_POINT('Ctrl Pts',(4.70524037260182,6.00000000093865,-67.4883108816615));
#7846=CARTESIAN_POINT('Ctrl Pts',(4.64516926942165,6.00000000081218,-67.4627166925166));
#7847=CARTESIAN_POINT('Ctrl Pts',(4.58494545881954,6.0000000006505,-67.4376372856515));
#7848=CARTESIAN_POINT('Ctrl Pts',(4.34284135212469,6.00000000000053,-67.3368162426988));
#7849=CARTESIAN_POINT('Ctrl Pts',(4.0981160083979,6.00000000028404,-67.2443422503418));
#7850=CARTESIAN_POINT('Ctrl Pts',(3.85139338320861,6.00000000163487,-67.1601340992298));
#7851=CARTESIAN_POINT('Ctrl Pts',(3.60459794198451,6.0000000029861,-67.0759010954977));
#7852=CARTESIAN_POINT('Ctrl Pts',(3.35580404208615,6.00000000623266,-66.9999387113475));
#7853=CARTESIAN_POINT('Ctrl Pts',(3.10471881286491,6.00000000804558,-66.9321924190084));
#7854=CARTESIAN_POINT('Ctrl Pts',(2.86855020564974,6.0000000097508,-66.8684708390678));
#7855=CARTESIAN_POINT('Ctrl Pts',(2.63069277643225,6.00000000585791,-66.8120699357947));
#7856=CARTESIAN_POINT('Ctrl Pts',(2.39076110075127,6.00000000323229,-66.7629601317855));
#7857=CARTESIAN_POINT('Ctrl Pts',(2.24875049531973,6.00000000167824,-66.7338930526673));
#7858=CARTESIAN_POINT('Ctrl Pts',(2.10601323548916,6.00000000066935,-66.7073812094719));
#7859=CARTESIAN_POINT('Ctrl Pts',(1.96246914678003,6.00000000028938,-66.6834270406419));
#7860=CARTESIAN_POINT('Ctrl Pts',(1.83293087812574,5.9999999999465,-66.6618101173314));
#7861=CARTESIAN_POINT('Ctrl Pts',(1.70273547973188,5.99999999999977,-66.6422761731934));
#7862=CARTESIAN_POINT('Ctrl Pts',(1.5720255845334,5.99999999999977,-66.6248804795373));
#7863=CARTESIAN_POINT('Ctrl Pts',(1.40616078506809,5.99999999999977,-66.6028061504634));
#7864=CARTESIAN_POINT('Ctrl Pts',(1.23927157998101,6.00000000003217,-66.5841437759783));
#7865=CARTESIAN_POINT('Ctrl Pts',(1.07202619547598,6.0000000000765,-66.5690240649954));
#7866=CARTESIAN_POINT('Ctrl Pts',(1.04376272367814,6.00000000008399,-66.5664689240794));
#7867=CARTESIAN_POINT('Ctrl Pts',(1.01548909646327,6.00000000009016,-66.5640148386483));
#7868=CARTESIAN_POINT('Ctrl Pts',(0.987208553067123,6.00000000009342,-66.5616622922949));
#7869=CARTESIAN_POINT('Ctrl Pts',(0.920377643541939,6.00000000010111,-66.5561028937254));
#7870=CARTESIAN_POINT('Ctrl Pts',(0.853508114226926,6.0000000000884,-66.5511106251358));
#7871=CARTESIAN_POINT('Ctrl Pts',(0.786635623670159,6.00000000005849,-66.546683494606));
#7872=CARTESIAN_POINT('Ctrl Pts',(0.595551811466195,5.99999999997304,-66.5340332557451));
#7873=CARTESIAN_POINT('Ctrl Pts',(0.404475822382095,5.99999999999819,-66.5260266785561));
#7874=CARTESIAN_POINT('Ctrl Pts',(0.213506141043386,6.00000000000357,-66.5226020043316));
#7875=CARTESIAN_POINT('Ctrl Pts',(0.143592221144975,6.00000000000553,-66.5213482325406));
#7876=CARTESIAN_POINT('Ctrl Pts',(0.0736925003305599,6.00000000000947,-66.520709072491));
#7877=CARTESIAN_POINT('Ctrl Pts',(0.00381174273192314,6.00000000002068,
-66.5206832338361));
#7878=CARTESIAN_POINT('Ctrl Pts',(0.00223179946017313,6.00000000002093,
-66.5206826496465));
#7879=CARTESIAN_POINT('Ctrl Pts',(0.000651865883589953,6.00000000002119,
-66.5206823790097));
#7880=CARTESIAN_POINT('Ctrl Pts',(-0.000928058234337155,6.00000000002145,
-66.5206824219519));
#7881=CARTESIAN_POINT('Ctrl Pts',(-0.263264677338428,6.00000000006482,-66.520689552242));
#7882=CARTESIAN_POINT('Ctrl Pts',(-0.525331339169259,6.00000000028711,-66.5293351560878));
#7883=CARTESIAN_POINT('Ctrl Pts',(-0.787710887408489,6.00000000019101,-66.5467414956877));
#7884=CARTESIAN_POINT('Ctrl Pts',(-0.851266591343311,6.00000000016774,-66.5509578005545));
#7885=CARTESIAN_POINT('Ctrl Pts',(-0.914818365061761,6.00000000013568,-66.5556874880789));
#7886=CARTESIAN_POINT('Ctrl Pts',(-0.978365706981233,6.00000000010664,-66.560931726518));
#7887=CARTESIAN_POINT('Ctrl Pts',(-1.17716339205941,6.00000000001582,-66.5773374868567));
#7888=CARTESIAN_POINT('Ctrl Pts',(-1.37591689807605,5.99999999999977,-66.5987815572106));
#7889=CARTESIAN_POINT('Ctrl Pts',(-1.57344188122075,5.99999999999977,-66.6250804427651));
#7890=CARTESIAN_POINT('Ctrl Pts',(-1.70144110734177,5.99999999999977,-66.6421225249627));
#7891=CARTESIAN_POINT('Ctrl Pts',(-1.82903601209464,5.99999999999399,-66.6612185682778));
#7892=CARTESIAN_POINT('Ctrl Pts',(-1.95599749600092,6.0000000000624,-66.6823299049636));
#7893=CARTESIAN_POINT('Ctrl Pts',(-2.08758818528542,6.0000000001333,-66.7042109925243));
#7894=CARTESIAN_POINT('Ctrl Pts',(-2.21849837114969,6.00000000030333,-66.7282569777027));
#7895=CARTESIAN_POINT('Ctrl Pts',(-2.34882467025348,6.00000000042092,-66.7544592401104));
#7896=CARTESIAN_POINT('Ctrl Pts',(-2.53816635487132,6.00000000059176,-66.7925266182157));
#7897=CARTESIAN_POINT('Ctrl Pts',(-2.72608639026754,6.00000000028953,-66.8350974685097));
#7898=CARTESIAN_POINT('Ctrl Pts',(-2.91266554092604,6.00000000015476,-66.8821207250386));
#7899=CARTESIAN_POINT('Ctrl Pts',(-2.97841818014486,6.00000000010727,-66.8986922616252));
#7900=CARTESIAN_POINT('Ctrl Pts',(-3.04400427898507,6.00000000007635,-66.9158166284133));
#7901=CARTESIAN_POINT('Ctrl Pts',(-3.10941746042439,6.00000000006051,-66.933492240734));
#7902=CARTESIAN_POINT('Ctrl Pts',(-3.35744519690348,6.00000000000045,-67.0005130157267));
#7903=CARTESIAN_POINT('Ctrl Pts',(-3.60321039549219,6.00000000000121,-67.0755019333164));
#7904=CARTESIAN_POINT('Ctrl Pts',(-3.84653444986901,6.00000000001263,-67.1583991671131));
#7905=CARTESIAN_POINT('Ctrl Pts',(-4.09574737289984,6.00000000002432,-67.2433026592835));
#7906=CARTESIAN_POINT('Ctrl Pts',(-4.34239946517691,5.99999999999479,-67.336501827309));
#7907=CARTESIAN_POINT('Ctrl Pts',(-4.58683540182128,6.00000000045564,-67.4383837794248));
#7908=CARTESIAN_POINT('Ctrl Pts',(-4.64389967612715,6.00000000056323,-67.4621684149501));
#7909=CARTESIAN_POINT('Ctrl Pts',(-4.70081907510701,6.00000000064926,-67.4864135837856));
#7910=CARTESIAN_POINT('Ctrl Pts',(-4.75761051430218,6.00000000070297,-67.5111290206764));
#7911=CARTESIAN_POINT('Ctrl Pts',(-4.91645120347176,6.00000000085317,-67.5802559363611));
#7912=CARTESIAN_POINT('Ctrl Pts',(-5.07429236532074,6.00000000074464,-67.6530582185577));
#7913=CARTESIAN_POINT('Ctrl Pts',(-5.23069101215385,6.00000000068362,-67.7293290427591));
#7914=CARTESIAN_POINT('Ctrl Pts',(-5.36954056109083,6.00000000062944,-67.7970417100477));
#7915=CARTESIAN_POINT('Ctrl Pts',(-5.50725375393251,6.00000000059421,-67.8674892809091));
#7916=CARTESIAN_POINT('Ctrl Pts',(-5.6434987472227,6.00000000084558,-67.9405537264822));
#7917=CARTESIAN_POINT('Ctrl Pts',(-5.76343389597552,6.00000000106685,-68.0048716506622));
#7918=CARTESIAN_POINT('Ctrl Pts',(-5.88223041979097,6.00000000143562,-68.0712175381268));
#7919=CARTESIAN_POINT('Ctrl Pts',(-6.00000000000007,6.00000000292373,-68.1396788547223));
#7920=CARTESIAN_POINT('',(-8.,5.99999999999995,-14.8323969741913));
#7921=CARTESIAN_POINT('Ctrl Pts',(-6.,5.99999999999994,-16.9705627484772));
#7922=CARTESIAN_POINT('Ctrl Pts',(-6.,5.99999999999994,-16.7029092618309));
#7923=CARTESIAN_POINT('Ctrl Pts',(-6.06020384677459,5.99999999999994,-16.3874179356908));
#7924=CARTESIAN_POINT('Ctrl Pts',(-6.25585405294364,5.99999999999994,-15.8960743911704));
#7925=CARTESIAN_POINT('Ctrl Pts',(-6.42385919064368,5.99999999999994,-15.6314481148128));
#7926=CARTESIAN_POINT('Ctrl Pts',(-6.7778910457933,5.99999999999995,-15.2614647616422));
#7927=CARTESIAN_POINT('Ctrl Pts',(-7.02372732242562,5.99999999999995,-15.0877073947429));
#7928=CARTESIAN_POINT('Ctrl Pts',(-7.47536381734142,5.99999999999995,-14.8921163084765));
#7929=CARTESIAN_POINT('Ctrl Pts',(-7.75869936772315,5.99999999999995,-14.8323969741913));
#7930=CARTESIAN_POINT('Ctrl Pts',(-8.,5.99999999999995,-14.8323969741913));
#7931=CARTESIAN_POINT('',(8.,5.99999999999995,-14.8323969741913));
#7932=CARTESIAN_POINT('',(8.,5.99999999999995,-14.8323969741913));
#7933=CARTESIAN_POINT('Ctrl Pts',(8.,5.99999999999995,-14.8323969741913));
#7934=CARTESIAN_POINT('Ctrl Pts',(7.75869936772315,5.99999999999995,-14.8323969741913));
#7935=CARTESIAN_POINT('Ctrl Pts',(7.47536381734142,5.99999999999995,-14.8921163084765));
#7936=CARTESIAN_POINT('Ctrl Pts',(7.02372732242562,5.99999999999995,-15.0877073947429));
#7937=CARTESIAN_POINT('Ctrl Pts',(6.7778910457933,5.99999999999995,-15.2614647616422));
#7938=CARTESIAN_POINT('Ctrl Pts',(6.42385919064368,5.99999999999994,-15.6314481148128));
#7939=CARTESIAN_POINT('Ctrl Pts',(6.25585405294364,5.99999999999994,-15.8960743911704));
#7940=CARTESIAN_POINT('Ctrl Pts',(6.06020384677459,5.99999999999994,-16.3874179356908));
#7941=CARTESIAN_POINT('Ctrl Pts',(6.,5.99999999999994,-16.7029092618309));
#7942=CARTESIAN_POINT('Ctrl Pts',(6.,5.99999999999994,-16.9705627484772));
#7943=CARTESIAN_POINT('Origin',(0.,-6.,2.09488880330588E-14));
#7944=CARTESIAN_POINT('Ctrl Pts',(-5.99997872967542,-6.00000000000024,-68.1397154447039));
#7945=CARTESIAN_POINT('Ctrl Pts',(-5.88065306094768,-6.00000000000024,-68.070356028456));
#7946=CARTESIAN_POINT('Ctrl Pts',(-5.76035179595835,-5.99999999978724,-68.0032029450616));
#7947=CARTESIAN_POINT('Ctrl Pts',(-5.63919789927778,-6.00000000114149,-67.938257741962));
#7948=CARTESIAN_POINT('Ctrl Pts',(-5.36452811515037,-6.00000000421175,-67.7910195151757));
#7949=CARTESIAN_POINT('Ctrl Pts',(-5.08547906226534,-6.00000002415142,-67.6551300980379));
#7950=CARTESIAN_POINT('Ctrl Pts',(-4.80172154724994,-6.00000003249791,-67.5303613497886));
#7951=CARTESIAN_POINT('Ctrl Pts',(-4.73247230274036,-6.00000003453481,-67.499912318142));
#7952=CARTESIAN_POINT('Ctrl Pts',(-4.66294239805607,-6.00000003545488,-67.4701255521591));
#7953=CARTESIAN_POINT('Ctrl Pts',(-4.59312657863782,-6.00000003465391,-67.4409976541893));
#7954=CARTESIAN_POINT('Ctrl Pts',(-4.39454299406212,-6.00000003237562,-67.358146483234));
#7955=CARTESIAN_POINT('Ctrl Pts',(-4.19396786917798,-6.00000002041265,-67.2807776472526));
#7956=CARTESIAN_POINT('Ctrl Pts',(-3.99105655262234,-6.00000001234683,-67.2087977787802));
#7957=CARTESIAN_POINT('Ctrl Pts',(-3.94543987688706,-6.00000001053355,-67.1926159197528));
#7958=CARTESIAN_POINT('Ctrl Pts',(-3.89970508733666,-6.00000000888316,-67.1767066229859));
#7959=CARTESIAN_POINT('Ctrl Pts',(-3.85384819076817,-6.0000000074552,-67.1610691807499));
#7960=CARTESIAN_POINT('Ctrl Pts',(-3.64869141653897,-6.00000000106674,-67.0911096447497));
#7961=CARTESIAN_POINT('Ctrl Pts',(-3.44109171841246,-6.00000000007894,-67.0265873650583));
#7962=CARTESIAN_POINT('Ctrl Pts',(-3.23159036684668,-6.00000000001056,-66.9676682583467));
#7963=CARTESIAN_POINT('Ctrl Pts',(-3.19055146412293,-5.99999999999717,-66.9561266836942));
#7964=CARTESIAN_POINT('Ctrl Pts',(-3.14943955853333,-6.00000000000023,-66.9448002727395));
#7965=CARTESIAN_POINT('Ctrl Pts',(-3.10825868593511,-6.00000000000023,-66.9336905046549));
#7966=CARTESIAN_POINT('Ctrl Pts',(-2.95466816752725,-6.00000000000023,-66.8922548834103));
#7967=CARTESIAN_POINT('Ctrl Pts',(-2.79997518606765,-6.00000000000023,-66.8537662550196));
#7968=CARTESIAN_POINT('Ctrl Pts',(-2.6448032490687,-6.00000000000023,-66.8183882438221));
#7969=CARTESIAN_POINT('Ctrl Pts',(-2.54365437995968,-6.00000000000023,-66.7953270776527));
#7970=CARTESIAN_POINT('Ctrl Pts',(-2.4423023734785,-6.00000000000023,-66.7735866407805));
#7971=CARTESIAN_POINT('Ctrl Pts',(-2.34092187223618,-6.00000000000023,-66.7532004707004));
#7972=CARTESIAN_POINT('Ctrl Pts',(-2.21137469343365,-6.00000000000023,-66.7271503842626));
#7973=CARTESIAN_POINT('Ctrl Pts',(-2.08172507159667,-5.99999999964996,-66.7033287187243));
#7974=CARTESIAN_POINT('Ctrl Pts',(-1.95199939961633,-6.00000000156985,-66.6817296203148));
#7975=CARTESIAN_POINT('Ctrl Pts',(-1.824463314101,-6.00000000345734,-66.6604950842376));
#7976=CARTESIAN_POINT('Ctrl Pts',(-1.69685357491418,-6.00000000797633,-66.6414087341013));
#7977=CARTESIAN_POINT('Ctrl Pts',(-1.56900071732305,-6.00000001702602,-66.6244302686289));
#7978=CARTESIAN_POINT('Ctrl Pts',(-1.33655492556664,-6.00000003347902,-66.5935621838328));
#7979=CARTESIAN_POINT('Ctrl Pts',(-1.10349609256449,-6.00000003523112,-66.5695462510003));
#7980=CARTESIAN_POINT('Ctrl Pts',(-0.869853272257425,-6.00000002613846,
-66.5524429803587));
#7981=CARTESIAN_POINT('Ctrl Pts',(-0.639795826763875,-6.00000001718533,
-66.5356021686093));
#7982=CARTESIAN_POINT('Ctrl Pts',(-0.409172035298845,-6.00000000564921,
-66.5254634964283));
#7983=CARTESIAN_POINT('Ctrl Pts',(-0.178031919006002,-6.00000000232865,
-66.5220391591688));
#7984=CARTESIAN_POINT('Ctrl Pts',(-0.123016782862887,-6.00000000153831,
-66.521224110775));
#7985=CARTESIAN_POINT('Ctrl Pts',(-0.0679725019716026,-6.00000000104546,
-66.5207892356362));
#7986=CARTESIAN_POINT('Ctrl Pts',(-0.0128999542220165,-6.00000000073503,
-66.5207343095857));
#7987=CARTESIAN_POINT('Ctrl Pts',(-0.012482287975762,-6.00000000073268,
-66.5207338930305));
#7988=CARTESIAN_POINT('Ctrl Pts',(-0.0120646200720832,-6.00000000073033,
-66.5207334982936));
#7989=CARTESIAN_POINT('Ctrl Pts',(-0.0116469505067236,-6.000000000728,-66.5207331253744));
#7990=CARTESIAN_POINT('Ctrl Pts',(0.169989366969348,-5.99999999971235,-66.5205709501121));
#7991=CARTESIAN_POINT('Ctrl Pts',(0.351939413797874,-6.00000000000218,-66.5245306974));
#7992=CARTESIAN_POINT('Ctrl Pts',(0.534215007419024,-6.00000000002061,-66.5326993242846));
#7993=CARTESIAN_POINT('Ctrl Pts',(0.613160572127682,-6.00000000002859,-66.5362372464468));
#7994=CARTESIAN_POINT('Ctrl Pts',(0.692167277879461,-6.00000000004884,-66.5405653421137));
#7995=CARTESIAN_POINT('Ctrl Pts',(0.771236245526539,-6.00000000012279,-66.5456937235993));
#7996=CARTESIAN_POINT('Ctrl Pts',(0.836809062903187,-6.00000000018411,-66.5499467501988));
#7997=CARTESIAN_POINT('Ctrl Pts',(0.902416572517938,-6.00000000023104,-66.5547456408318));
#7998=CARTESIAN_POINT('Ctrl Pts',(0.96802849280209,-6.00000000024428,-66.5600951583082));
#7999=CARTESIAN_POINT('Ctrl Pts',(1.13715461784052,-6.00000000027841,-66.5738844691179));
#8000=CARTESIAN_POINT('Ctrl Pts',(1.3063098085867,-6.00000000012487,-66.5913360753138));
#8001=CARTESIAN_POINT('Ctrl Pts',(1.47473506099623,-6.00000000007166,-66.6123416933938));
#8002=CARTESIAN_POINT('Ctrl Pts',(1.50208873361841,-6.00000000006302,-66.6157531818254));
#8003=CARTESIAN_POINT('Ctrl Pts',(1.52942316435998,-6.00000000005606,-66.6192583016056));
#8004=CARTESIAN_POINT('Ctrl Pts',(1.55673512158337,-6.00000000005077,-66.6228564609117));
#8005=CARTESIAN_POINT('Ctrl Pts',(1.68662492850993,-6.00000000002558,-66.6399685343434));
#8006=CARTESIAN_POINT('Ctrl Pts',(1.81617214090643,-6.0000000000153,-66.6592036204614));
#8007=CARTESIAN_POINT('Ctrl Pts',(1.94516884575325,-6.00000000000929,-66.6805232592598));
#8008=CARTESIAN_POINT('Ctrl Pts',(2.26860782880832,-5.99999999999422,-66.7339789060551));
#8009=CARTESIAN_POINT('Ctrl Pts',(2.58858611930201,-6.00000000000024,-66.8005396713465));
#8010=CARTESIAN_POINT('Ctrl Pts',(2.9066523490031,-6.00000000000024,-66.8805814871616));
#8011=CARTESIAN_POINT('Ctrl Pts',(2.97098604581056,-6.00000000000024,-66.8967711528026));
#8012=CARTESIAN_POINT('Ctrl Pts',(3.0352415115127,-6.00000000000024,-66.9135123439025));
#8013=CARTESIAN_POINT('Ctrl Pts',(3.0993837879325,-6.00000000000024,-66.9307945087936));
#8014=CARTESIAN_POINT('Ctrl Pts',(3.35209374305792,-6.00000000000024,-66.9988833786916));
#8015=CARTESIAN_POINT('Ctrl Pts',(3.60338827102687,-5.99999999998588,-67.0754603115548));
#8016=CARTESIAN_POINT('Ctrl Pts',(3.85114437890632,-6.0000000000146,-67.159971681504));
#8017=CARTESIAN_POINT('Ctrl Pts',(3.85228098497779,-6.00000000001474,-67.1603593859163));
#8018=CARTESIAN_POINT('Ctrl Pts',(3.85341751650643,-6.00000000001487,-67.1607472573209));
#8019=CARTESIAN_POINT('Ctrl Pts',(3.85455397349793,-6.000000000015,-67.1611352957054));
#8020=CARTESIAN_POINT('Ctrl Pts',(4.10341404208677,-6.00000000004453,-67.2461075029162));
#8021=CARTESIAN_POINT('Ctrl Pts',(4.34869348585104,-6.00000000022622,-67.3390831996519));
#8022=CARTESIAN_POINT('Ctrl Pts',(4.59052929362912,-6.00000000011317,-67.4399236158872));
#8023=CARTESIAN_POINT('Ctrl Pts',(4.6483342431954,-6.00000000008615,-67.464027057095));
#8024=CARTESIAN_POINT('Ctrl Pts',(4.70594363997126,-6.00000000006834,-67.4885826241901));
#8025=CARTESIAN_POINT('Ctrl Pts',(4.763357441056,-6.0000000000555,-67.513588419992));
#8026=CARTESIAN_POINT('Ctrl Pts',(5.06065596138665,-5.99999999998898,-67.6430727243079));
#8027=CARTESIAN_POINT('Ctrl Pts',(5.35270991438456,-6.00000000000393,-67.7846295793901));
#8028=CARTESIAN_POINT('Ctrl Pts',(5.63934396309719,-6.00000000004665,-67.9382748405765));
#8029=CARTESIAN_POINT('Ctrl Pts',(5.76052186835046,-6.0000000000647,-68.0032301764352));
#8030=CARTESIAN_POINT('Ctrl Pts',(5.8807310423892,-6.00000000009423,-68.0703459263676));
#8031=CARTESIAN_POINT('Ctrl Pts',(5.99999999999997,-6.00000000014129,-68.1396788547224));
#8032=CARTESIAN_POINT('',(8.,-6.00000000000005,-14.8323969741913));
#8033=CARTESIAN_POINT('Ctrl Pts',(6.,-6.00000000000006,-16.9705627484771));
#8034=CARTESIAN_POINT('Ctrl Pts',(6.,-6.00000000000006,-16.7029092618308));
#8035=CARTESIAN_POINT('Ctrl Pts',(6.06020384677459,-6.00000000000006,-16.3874179356908));
#8036=CARTESIAN_POINT('Ctrl Pts',(6.25585405294365,-6.00000000000006,-15.8960743911704));
#8037=CARTESIAN_POINT('Ctrl Pts',(6.42385919064368,-6.00000000000006,-15.6314481148128));
#8038=CARTESIAN_POINT('Ctrl Pts',(6.7778910457933,-6.00000000000005,-15.2614647616422));
#8039=CARTESIAN_POINT('Ctrl Pts',(7.02372732242562,-6.00000000000005,-15.0877073947429));
#8040=CARTESIAN_POINT('Ctrl Pts',(7.47536381734142,-6.00000000000005,-14.8921163084765));
#8041=CARTESIAN_POINT('Ctrl Pts',(7.75869936772315,-6.00000000000005,-14.8323969741913));
#8042=CARTESIAN_POINT('Ctrl Pts',(8.,-6.00000000000005,-14.8323969741913));
#8043=CARTESIAN_POINT('',(-8.,-6.00000000000005,-14.8323969741913));
#8044=CARTESIAN_POINT('',(8.,-6.00000000000005,-14.8323969741913));
#8045=CARTESIAN_POINT('Ctrl Pts',(-8.,-6.00000000000005,-14.8323969741913));
#8046=CARTESIAN_POINT('Ctrl Pts',(-7.75869936772315,-6.00000000000005,-14.8323969741913));
#8047=CARTESIAN_POINT('Ctrl Pts',(-7.47536381734142,-6.00000000000005,-14.8921163084765));
#8048=CARTESIAN_POINT('Ctrl Pts',(-7.02372732242562,-6.00000000000005,-15.0877073947429));
#8049=CARTESIAN_POINT('Ctrl Pts',(-6.7778910457933,-6.00000000000005,-15.2614647616422));
#8050=CARTESIAN_POINT('Ctrl Pts',(-6.42385919064368,-6.00000000000006,-15.6314481148128));
#8051=CARTESIAN_POINT('Ctrl Pts',(-6.25585405294364,-6.00000000000006,-15.8960743911704));
#8052=CARTESIAN_POINT('Ctrl Pts',(-6.06020384677459,-6.00000000000006,-16.3874179356908));
#8053=CARTESIAN_POINT('Ctrl Pts',(-6.,-6.00000000000006,-16.7029092618308));
#8054=CARTESIAN_POINT('Ctrl Pts',(-6.,-6.00000000000006,-16.9705627484771));
#8055=CARTESIAN_POINT('Origin',(0.,6.,-2.09488880330588E-14));
#8056=CARTESIAN_POINT('',(5.99999160300743,6.00000000000024,68.1397295132015));
#8057=CARTESIAN_POINT('Ctrl Pts',(-5.99999999999999,6.00000000023105,68.1396788547224));
#8058=CARTESIAN_POINT('Ctrl Pts',(-5.88444358312955,6.00000000011434,68.0725115980034));
#8059=CARTESIAN_POINT('Ctrl Pts',(-5.76789237998722,6.00000000006755,68.0073544868762));
#8060=CARTESIAN_POINT('Ctrl Pts',(-5.65036932229242,6.00000000004037,67.9441916161475));
#8061=CARTESIAN_POINT('Ctrl Pts',(-5.3873288140795,5.99999999997953,67.8028202636442));
#8062=CARTESIAN_POINT('Ctrl Pts',(-5.1194177726107,6.0000000000003,67.6714423841422));
#8063=CARTESIAN_POINT('Ctrl Pts',(-4.84664783679216,6.00000000000025,67.5502106840568));
#8064=CARTESIAN_POINT('Ctrl Pts',(-4.82125130085735,6.00000000000024,67.5389232772595));
#8065=CARTESIAN_POINT('Ctrl Pts',(-4.79581266378767,6.00000000000024,67.5277237930512));
#8066=CARTESIAN_POINT('Ctrl Pts',(-4.77033194696672,6.00000000000024,67.5166123348889));
#8067=CARTESIAN_POINT('Ctrl Pts',(-4.70876721194481,6.00000000000023,67.4897656028181));
#8068=CARTESIAN_POINT('Ctrl Pts',(-4.64695686427904,6.00000000000024,67.463432758374));
#8069=CARTESIAN_POINT('Ctrl Pts',(-4.5849461772848,6.00000000000024,67.4376274899832));
#8070=CARTESIAN_POINT('Ctrl Pts',(-4.38827148386229,6.00000000000024,67.3557828355303));
#8071=CARTESIAN_POINT('Ctrl Pts',(-4.18925929943197,5.9999999999863,67.2791062947266));
#8072=CARTESIAN_POINT('Ctrl Pts',(-3.98903483489981,6.00000000001416,67.2080000447656));
#8073=CARTESIAN_POINT('Ctrl Pts',(-3.94362722082296,6.00000000002047,67.1918743172517));
#8074=CARTESIAN_POINT('Ctrl Pts',(-3.8981571587602,6.00000000003015,67.1760352619909));
#8075=CARTESIAN_POINT('Ctrl Pts',(-3.85263764092992,6.00000000004771,67.1604879161245));
#8076=CARTESIAN_POINT('Ctrl Pts',(-3.85062837020849,6.00000000004849,67.1598016428876));
#8077=CARTESIAN_POINT('Ctrl Pts',(-3.84861900312364,6.00000000004928,67.1591159380443));
#8078=CARTESIAN_POINT('Ctrl Pts',(-3.84660953923603,6.00000000005009,67.1584308013561));
#8079=CARTESIAN_POINT('Ctrl Pts',(-3.59833898175711,6.00000000014983,67.0737817222825));
#8080=CARTESIAN_POINT('Ctrl Pts',(-3.34861996632779,6.00000000048239,66.9978044385423));
#8081=CARTESIAN_POINT('Ctrl Pts',(-3.0970540533494,6.00000000024139,66.9301379860738));
#8082=CARTESIAN_POINT('Ctrl Pts',(-3.03681722293726,6.00000000018369,66.9139354228025));
#8083=CARTESIAN_POINT('Ctrl Pts',(-2.97647791034341,6.00000000014616,66.8982129891066));
#8084=CARTESIAN_POINT('Ctrl Pts',(-2.91603033355864,6.00000000011925,66.8829659566196));
#8085=CARTESIAN_POINT('Ctrl Pts',(-2.60112596601868,5.99999999997907,66.8035358557358));
#8086=CARTESIAN_POINT('Ctrl Pts',(-2.28328401837121,6.00000000001375,66.7370060636242));
#8087=CARTESIAN_POINT('Ctrl Pts',(-1.96277620531409,6.00000000011972,66.6834659686194));
#8088=CARTESIAN_POINT('Ctrl Pts',(-1.83093099886256,6.00000000016332,66.6614415293022));
#8089=CARTESIAN_POINT('Ctrl Pts',(-1.69863458891165,6.00000000023189,66.6416154643382));
#8090=CARTESIAN_POINT('Ctrl Pts',(-1.56583784127881,6.00000000033247,66.6240105759369));
#8091=CARTESIAN_POINT('Ctrl Pts',(-1.37578755107881,6.0000000004764,66.5988155752367));
#8092=CARTESIAN_POINT('Ctrl Pts',(-1.18485631346681,6.00000000006835,66.5781555766083));
#8093=CARTESIAN_POINT('Ctrl Pts',(-0.992844141885393,6.00000000001632,66.5621208184677));
#8094=CARTESIAN_POINT('Ctrl Pts',(-0.923392355514658,5.99999999999751,66.5563209642829));
#8095=CARTESIAN_POINT('Ctrl Pts',(-0.853799205652419,6.00000000000023,66.5511263631302));
#8096=CARTESIAN_POINT('Ctrl Pts',(-0.784105240804896,6.00000000000023,66.5465412829041));
#8097=CARTESIAN_POINT('Ctrl Pts',(-0.557169468556095,6.00000000000023,66.5316114575713));
#8098=CARTESIAN_POINT('Ctrl Pts',(-0.328878073721691,6.00000000002498,66.5231044417488));
#8099=CARTESIAN_POINT('Ctrl Pts',(-0.100972736629075,6.0000000000241,66.521128825034));
#8100=CARTESIAN_POINT('Ctrl Pts',(-0.0701670299566568,6.00000000002398,
66.520861783157));
#8101=CARTESIAN_POINT('Ctrl Pts',(-0.0393683869893167,6.00000000002292,
66.52071399686));
#8102=CARTESIAN_POINT('Ctrl Pts',(-0.00858111222863268,6.0000000000209,
66.5206856616905));
#8103=CARTESIAN_POINT('Ctrl Pts',(-0.00379835720684805,6.00000000002059,
66.5206812598662));
#8104=CARTESIAN_POINT('Ctrl Pts',(0.000984123469690708,6.00000000002025,
66.5206797407381));
#8105=CARTESIAN_POINT('Ctrl Pts',(0.00576633055906461,6.0000000000199,66.5206811037694));
#8106=CARTESIAN_POINT('Ctrl Pts',(0.234106652522432,6.00000000000284,66.5207461856436));
#8107=CARTESIAN_POINT('Ctrl Pts',(0.461569701198186,6.00000000000127,66.5273927740508));
#8108=CARTESIAN_POINT('Ctrl Pts',(0.688691383104901,6.00000000000606,66.540566912047));
#8109=CARTESIAN_POINT('Ctrl Pts',(0.783642201262397,6.00000000000806,66.5460745111928));
#8110=CARTESIAN_POINT('Ctrl Pts',(0.8785332758493,6.00000000001171,66.5527235909363));
#8111=CARTESIAN_POINT('Ctrl Pts',(0.97340352404493,6.00000000002363,66.5605128893986));
#8112=CARTESIAN_POINT('Ctrl Pts',(1.17496698405461,6.00000000004895,66.5770622078518));
#8113=CARTESIAN_POINT('Ctrl Pts',(1.37643687431007,6.00000000008962,66.5987564371885));
#8114=CARTESIAN_POINT('Ctrl Pts',(1.57748427575531,6.00000000038885,66.625614231632));
#8115=CARTESIAN_POINT('Ctrl Pts',(1.70189213807276,6.00000000057401,66.6422337988051));
#8116=CARTESIAN_POINT('Ctrl Pts',(1.82623013085954,6.00000000051554,66.6608311538313));
#8117=CARTESIAN_POINT('Ctrl Pts',(1.95020071616002,6.00000000038028,66.6813903002302));
#8118=CARTESIAN_POINT('Ctrl Pts',(2.08632406742112,6.00000000023175,66.7039648480563));
#8119=CARTESIAN_POINT('Ctrl Pts',(2.22200401493324,6.00000000007876,66.728905060495));
#8120=CARTESIAN_POINT('Ctrl Pts',(2.35681175916437,6.0000000000386,66.7560991155276));
#8121=CARTESIAN_POINT('Ctrl Pts',(2.5182845660602,5.99999999999049,66.7886721729735));
#8122=CARTESIAN_POINT('Ctrl Pts',(2.67856245718989,5.99999999999813,66.8244779431868));
#8123=CARTESIAN_POINT('Ctrl Pts',(2.83763002040604,6.00000000000674,66.8634569456343));
#8124=CARTESIAN_POINT('Ctrl Pts',(2.86242940696275,6.00000000000808,66.8695339567467));
#8125=CARTESIAN_POINT('Ctrl Pts',(2.88719934806261,6.00000000001001,66.8756881967657));
#8126=CARTESIAN_POINT('Ctrl Pts',(2.91193975118787,6.000000000013,66.8819195489396));
#8127=CARTESIAN_POINT('Ctrl Pts',(2.98164995633899,6.00000000002142,66.8994774212269));
#8128=CARTESIAN_POINT('Ctrl Pts',(3.05112570223683,6.00000000003702,66.917647375163));
#8129=CARTESIAN_POINT('Ctrl Pts',(3.12039979918319,6.00000000008208,66.9364364740021));
#8130=CARTESIAN_POINT('Ctrl Pts',(3.36532889442497,6.0000000002414,67.0028681877584));
#8131=CARTESIAN_POINT('Ctrl Pts',(3.60744466828179,6.00000000026126,67.076928038554));
#8132=CARTESIAN_POINT('Ctrl Pts',(3.84690034723213,6.00000000016467,67.1585433863136));
#8133=CARTESIAN_POINT('Ctrl Pts',(4.09931403384456,6.00000000006285,67.2445753021256));
#8134=CARTESIAN_POINT('Ctrl Pts',(4.34877192834515,6.00000000000415,67.3390031462041));
#8135=CARTESIAN_POINT('Ctrl Pts',(4.59510054381638,6.00000000000216,67.441825521795));
#8136=CARTESIAN_POINT('Ctrl Pts',(4.64870191485623,6.00000000000173,67.4641997810532));
#8137=CARTESIAN_POINT('Ctrl Pts',(4.70214519753807,6.00000000000142,67.4869664961653));
#8138=CARTESIAN_POINT('Ctrl Pts',(4.75543960720073,6.00000000000118,67.51012947957));
#8139=CARTESIAN_POINT('Ctrl Pts',(4.92114531381994,6.00000000000044,67.5821490132658));
#8140=CARTESIAN_POINT('Ctrl Pts',(5.08541305952541,6.00000000000035,67.6579958213788));
#8141=CARTESIAN_POINT('Ctrl Pts',(5.24831190515484,6.00000000000029,67.7377664886393));
#8142=CARTESIAN_POINT('Ctrl Pts',(5.37886967950357,6.00000000000024,67.8016999114673));
#8143=CARTESIAN_POINT('Ctrl Pts',(5.50854794803044,6.00000000000024,67.8681547506109));
#8144=CARTESIAN_POINT('Ctrl Pts',(5.63737298287251,6.00000000000024,67.9372030795001));
#8145=CARTESIAN_POINT('Ctrl Pts',(5.75906631496535,6.00000000000024,68.0024289203335));
#8146=CARTESIAN_POINT('Ctrl Pts',(5.87999873423005,6.00000000000024,68.0699695887378));
#8147=CARTESIAN_POINT('Ctrl Pts',(5.9999748090223,6.00000000000024,68.139722189381));
#8148=CARTESIAN_POINT('',(6.,6.00000000000006,16.9705627484771));
#8149=CARTESIAN_POINT('',(6.,6.00000000000024,68.1396788547224));
#8150=CARTESIAN_POINT('',(8.,6.00000000000005,14.8323969741913));
#8151=CARTESIAN_POINT('Ctrl Pts',(6.,6.00000000000006,16.9705627484771));
#8152=CARTESIAN_POINT('Ctrl Pts',(6.,6.00000000000006,16.7029092618308));
#8153=CARTESIAN_POINT('Ctrl Pts',(6.06020384677459,6.00000000000006,16.3874179356908));
#8154=CARTESIAN_POINT('Ctrl Pts',(6.25585405294364,6.00000000000006,15.8960743911704));
#8155=CARTESIAN_POINT('Ctrl Pts',(6.42385919064368,6.00000000000006,15.6314481148128));
#8156=CARTESIAN_POINT('Ctrl Pts',(6.7778910457933,6.00000000000005,15.2614647616422));
#8157=CARTESIAN_POINT('Ctrl Pts',(7.02372732242562,6.00000000000005,15.0877073947429));
#8158=CARTESIAN_POINT('Ctrl Pts',(7.47536381734142,6.00000000000005,14.8921163084765));
#8159=CARTESIAN_POINT('Ctrl Pts',(7.75869936772315,6.00000000000005,14.8323969741913));
#8160=CARTESIAN_POINT('Ctrl Pts',(8.,6.00000000000005,14.8323969741913));
#8161=CARTESIAN_POINT('',(-8.,6.00000000000005,14.8323969741913));
#8162=CARTESIAN_POINT('',(8.,6.00000000000005,14.8323969741913));
#8163=CARTESIAN_POINT('Ctrl Pts',(-8.,6.00000000000005,14.8323969741913));
#8164=CARTESIAN_POINT('Ctrl Pts',(-7.75869936772315,6.00000000000005,14.8323969741913));
#8165=CARTESIAN_POINT('Ctrl Pts',(-7.47536381734142,6.00000000000005,14.8921163084765));
#8166=CARTESIAN_POINT('Ctrl Pts',(-7.02372732242562,6.00000000000005,15.0877073947429));
#8167=CARTESIAN_POINT('Ctrl Pts',(-6.7778910457933,6.00000000000005,15.2614647616422));
#8168=CARTESIAN_POINT('Ctrl Pts',(-6.42385919064368,6.00000000000006,15.6314481148128));
#8169=CARTESIAN_POINT('Ctrl Pts',(-6.25585405294364,6.00000000000006,15.8960743911704));
#8170=CARTESIAN_POINT('Ctrl Pts',(-6.06020384677459,6.00000000000006,16.3874179356908));
#8171=CARTESIAN_POINT('Ctrl Pts',(-6.,6.00000000000006,16.7029092618308));
#8172=CARTESIAN_POINT('Ctrl Pts',(-6.,6.00000000000006,16.9705627484771));
#8173=CARTESIAN_POINT('Origin',(0.,-6.,2.09488880330588E-14));
#8174=CARTESIAN_POINT('',(6.,-5.99999999999976,68.1396788547224));
#8175=CARTESIAN_POINT('',(6.,-5.99999999999994,16.9705627484772));
#8176=CARTESIAN_POINT('',(6.,-5.99999999999976,68.1396788547224));
#8177=CARTESIAN_POINT('Ctrl Pts',(6.,-6.00000000024154,68.1396788547224));
#8178=CARTESIAN_POINT('Ctrl Pts',(5.88187316617764,-6.00000000015773,68.0710098609603));
#8179=CARTESIAN_POINT('Ctrl Pts',(5.76283444829439,-6.00000000010713,68.0045242065892));
#8180=CARTESIAN_POINT('Ctrl Pts',(5.64284459885907,-6.00000000007621,67.9401565816466));
#8181=CARTESIAN_POINT('Ctrl Pts',(5.35619790196524,-6.00000000000233,67.7863871822888));
#8182=CARTESIAN_POINT('Ctrl Pts',(5.06412377906966,-5.99999999998375,67.6447057808939));
#8183=CARTESIAN_POINT('Ctrl Pts',(4.76688742341354,-6.00000000007952,67.5151296844279));
#8184=CARTESIAN_POINT('Ctrl Pts',(4.70839720439327,-6.00000000009837,67.4896316788244));
#8185=CARTESIAN_POINT('Ctrl Pts',(4.64970707509721,-6.00000000012467,67.4646024152188));
#8186=CARTESIAN_POINT('Ctrl Pts',(4.5908152128972,-6.00000000016496,67.4400433025996));
#8187=CARTESIAN_POINT('Ctrl Pts',(4.34910031027361,-6.00000000033032,67.3392432379812));
#8188=CARTESIAN_POINT('Ctrl Pts',(4.10398677156061,-6.00000000008324,67.2463175761735));
#8189=CARTESIAN_POINT('Ctrl Pts',(3.85519952238743,-6.0000000000276,67.1613594452035));
#8190=CARTESIAN_POINT('Ctrl Pts',(3.85519100898521,-6.0000000000276,67.1613565379696));
#8191=CARTESIAN_POINT('Ctrl Pts',(3.85518249557866,-6.0000000000276,67.1613536307449));
#8192=CARTESIAN_POINT('Ctrl Pts',(3.85517398216783,-6.0000000000276,67.1613507235296));
#8193=CARTESIAN_POINT('Ctrl Pts',(3.60637796813298,-5.99999999997196,67.0763902308312));
#8194=CARTESIAN_POINT('Ctrl Pts',(3.35390683475957,-5.99999999999977,66.9994050968271));
#8195=CARTESIAN_POINT('Ctrl Pts',(3.10045926892741,-5.99999999999977,66.9310858798008));
#8196=CARTESIAN_POINT('Ctrl Pts',(3.03765054448378,-5.99999999999977,66.9141551870071));
#8197=CARTESIAN_POINT('Ctrl Pts',(2.97474929840994,-5.99999999999977,66.8977478662036));
#8198=CARTESIAN_POINT('Ctrl Pts',(2.9117977058822,-5.99999999999977,66.8818763978451));
#8199=CARTESIAN_POINT('Ctrl Pts',(2.6451072621979,-5.99999999999977,66.8146379250998));
#8200=CARTESIAN_POINT('Ctrl Pts',(2.37751303071259,-5.99999999999977,66.7570207931097));
#8201=CARTESIAN_POINT('Ctrl Pts',(2.1087222951943,-5.99999999999977,66.7087297576867));
#8202=CARTESIAN_POINT('Ctrl Pts',(2.05784880463699,-5.99999999999977,66.6995898089832));
#8203=CARTESIAN_POINT('Ctrl Pts',(2.00693246700169,-5.99999999999977,66.6907837938054));
#8204=CARTESIAN_POINT('Ctrl Pts',(1.95597132257835,-5.99999999999977,66.682309504294));
#8205=CARTESIAN_POINT('Ctrl Pts',(1.82681153224339,-5.99999999999977,66.6608316220973));
#8206=CARTESIAN_POINT('Ctrl Pts',(1.69736390198919,-5.99999999999977,66.6414847915479));
#8207=CARTESIAN_POINT('Ctrl Pts',(1.56767188528546,-5.99999999999977,66.6242743320315));
#8208=CARTESIAN_POINT('Ctrl Pts',(1.37574506873217,-5.99999999999977,66.5988051567472));
#8209=CARTESIAN_POINT('Ctrl Pts',(1.1831562426598,-5.99999999999976,66.5779992309698));
#8210=CARTESIAN_POINT('Ctrl Pts',(0.989984156733664,-6.00000000000307,66.561877611386));
#8211=CARTESIAN_POINT('Ctrl Pts',(0.666428323474948,-6.00000000000862,66.5348745170574));
#8212=CARTESIAN_POINT('Ctrl Pts',(0.34123645744333,-6.00000000001651,66.5210135615664));
#8213=CARTESIAN_POINT('Ctrl Pts',(0.0138227741859248,-6.00000000000467,
66.520685928579));
#8214=CARTESIAN_POINT('Ctrl Pts',(0.0121440744646398,-6.00000000000462,
66.5206842487548));
#8215=CARTESIAN_POINT('Ctrl Pts',(0.0104653163290937,-6.00000000000456,
66.5206829246754));
#8216=CARTESIAN_POINT('Ctrl Pts',(0.00878650039514419,-6.0000000000045,
66.5206819563299));
#8217=CARTESIAN_POINT('Ctrl Pts',(-0.253515514778501,-5.99999999999504,
66.5205306598399));
#8218=CARTESIAN_POINT('Ctrl Pts',(-0.517155929846906,-5.99999999999977,
66.5290771486489));
#8219=CARTESIAN_POINT('Ctrl Pts',(-0.779619496371868,-5.99999999999977,
66.5462435242154));
#8220=CARTESIAN_POINT('Ctrl Pts',(-0.843154223039775,-5.99999999999977,
66.5503989999408));
#8221=CARTESIAN_POINT('Ctrl Pts',(-0.906642860018819,-5.99999999999672,
66.5550642741598));
#8222=CARTESIAN_POINT('Ctrl Pts',(-0.970048401227494,-6.00000000001686,
66.5602369336203));
#8223=CARTESIAN_POINT('Ctrl Pts',(-1.16857275813673,-6.00000000007993,66.5764326615223));
#8224=CARTESIAN_POINT('Ctrl Pts',(-1.36628126414112,-6.00000000065265,66.5976041035957));
#8225=CARTESIAN_POINT('Ctrl Pts',(-1.56326721620696,-6.00000000036765,66.6236701056625));
#8226=CARTESIAN_POINT('Ctrl Pts',(-1.69082862701755,-6.0000000001831,66.640549563121));
#8227=CARTESIAN_POINT('Ctrl Pts',(-1.81800947701284,-6.00000000008209,66.6594883967265));
#8228=CARTESIAN_POINT('Ctrl Pts',(-1.9449607332334,-6.00000000004002,66.6804955904311));
#8229=CARTESIAN_POINT('Ctrl Pts',(-2.07666646789127,-5.99999999999637,66.7022895290052));
#8230=CARTESIAN_POINT('Ctrl Pts',(-2.20812514567989,-5.9999999999997,66.726309580931));
#8231=CARTESIAN_POINT('Ctrl Pts',(-2.33930748785715,-6.00000000000362,66.7525690041408));
#8232=CARTESIAN_POINT('Ctrl Pts',(-2.51361784999643,-6.00000000000884,66.7874615780445));
#8233=CARTESIAN_POINT('Ctrl Pts',(-2.68751489304227,-6.00000000005027,66.8263240896056));
#8234=CARTESIAN_POINT('Ctrl Pts',(-2.86039613598336,-6.00000000005924,66.8690635323667));
#8235=CARTESIAN_POINT('Ctrl Pts',(-2.87627884399349,-6.00000000006006,66.8729900317274));
#8236=CARTESIAN_POINT('Ctrl Pts',(-2.89215298635632,-6.00000000006047,66.8769492176875));
#8237=CARTESIAN_POINT('Ctrl Pts',(-2.90801810128637,-6.00000000006037,66.8809409966382));
#8238=CARTESIAN_POINT('Ctrl Pts',(-2.97469708400514,-6.00000000005998,66.8977179163669));
#8239=CARTESIAN_POINT('Ctrl Pts',(-3.04121657240003,-6.00000000004897,66.9150706470321));
#8240=CARTESIAN_POINT('Ctrl Pts',(-3.10753849583247,-6.00000000003208,66.9329830086901));
#8241=CARTESIAN_POINT('Ctrl Pts',(-3.28869151080579,-5.99999999998595,66.9819091880242));
#8242=CARTESIAN_POINT('Ctrl Pts',(-3.46839021870641,-5.9999999999722,67.0350304856278));
#8243=CARTESIAN_POINT('Ctrl Pts',(-3.64644665283845,-6.0000000000327,67.0922158714817));
#8244=CARTESIAN_POINT('Ctrl Pts',(-3.71447004547011,-6.00000000005581,67.1140625628057));
#8245=CARTESIAN_POINT('Ctrl Pts',(-3.78225355303331,-6.00000000009765,67.1365029097764));
#8246=CARTESIAN_POINT('Ctrl Pts',(-3.84978580544277,-6.00000000021853,67.1595314065013));
#8247=CARTESIAN_POINT('Ctrl Pts',(-3.85320864030556,-6.00000000022466,67.1606985931213));
#8248=CARTESIAN_POINT('Ctrl Pts',(-3.85663082958527,-6.000000000231,67.1618672908473));
#8249=CARTESIAN_POINT('Ctrl Pts',(-3.86005237553686,-6.00000000023757,67.1630375006439));
#8250=CARTESIAN_POINT('Ctrl Pts',(-4.10768501554717,-6.00000000071298,67.2477308367549));
#8251=CARTESIAN_POINT('Ctrl Pts',(-4.35191715526809,-6.00000000647157,67.3403748233525));
#8252=CARTESIAN_POINT('Ctrl Pts',(-4.59293426136656,-6.00000000770409,67.4409174182992));
#8253=CARTESIAN_POINT('Ctrl Pts',(-4.87724480016224,-6.00000000915801,67.5595202834814));
#8254=CARTESIAN_POINT('Ctrl Pts',(-5.15698013686088,-6.00000000332805,67.6891171054417));
#8255=CARTESIAN_POINT('Ctrl Pts',(-5.43224533975829,-6.0000000013192,67.8298568940711));
#8256=CARTESIAN_POINT('Ctrl Pts',(-5.50008164654291,-6.00000000082414,67.8645407821099));
#8257=CARTESIAN_POINT('Ctrl Pts',(-5.56764646050735,-6.00000000049553,67.8999011651933));
#8258=CARTESIAN_POINT('Ctrl Pts',(-5.63494133399271,-6.00000000030077,67.9359397796821));
#8259=CARTESIAN_POINT('Ctrl Pts',(-5.75755164084124,-5.99999999994593,68.0016016251097));
#8260=CARTESIAN_POINT('Ctrl Pts',(-5.8792658872803,-5.99999999999976,68.0695150849564));
#8261=CARTESIAN_POINT('Ctrl Pts',(-5.99999401150366,-5.99999999999976,68.1396891563318));
#8262=CARTESIAN_POINT('',(-8.,-5.99999999999995,14.8323969741913));
#8263=CARTESIAN_POINT('Ctrl Pts',(-6.,-5.99999999999994,16.9705627484772));
#8264=CARTESIAN_POINT('Ctrl Pts',(-6.,-5.99999999999994,16.7029092618309));
#8265=CARTESIAN_POINT('Ctrl Pts',(-6.06020384677459,-5.99999999999994,16.3874179356908));
#8266=CARTESIAN_POINT('Ctrl Pts',(-6.25585405294364,-5.99999999999994,15.8960743911704));
#8267=CARTESIAN_POINT('Ctrl Pts',(-6.42385919064368,-5.99999999999994,15.6314481148128));
#8268=CARTESIAN_POINT('Ctrl Pts',(-6.7778910457933,-5.99999999999995,15.2614647616422));
#8269=CARTESIAN_POINT('Ctrl Pts',(-7.02372732242562,-5.99999999999995,15.0877073947429));
#8270=CARTESIAN_POINT('Ctrl Pts',(-7.47536381734142,-5.99999999999995,14.8921163084765));
#8271=CARTESIAN_POINT('Ctrl Pts',(-7.75869936772315,-5.99999999999995,14.8323969741913));
#8272=CARTESIAN_POINT('Ctrl Pts',(-8.,-5.99999999999995,14.8323969741913));
#8273=CARTESIAN_POINT('',(8.,-5.99999999999995,14.8323969741913));
#8274=CARTESIAN_POINT('',(8.,-5.99999999999995,14.8323969741913));
#8275=CARTESIAN_POINT('Ctrl Pts',(8.,-5.99999999999995,14.8323969741913));
#8276=CARTESIAN_POINT('Ctrl Pts',(7.75869936772315,-5.99999999999995,14.8323969741913));
#8277=CARTESIAN_POINT('Ctrl Pts',(7.47536381734142,-5.99999999999995,14.8921163084765));
#8278=CARTESIAN_POINT('Ctrl Pts',(7.02372732242562,-5.99999999999995,15.0877073947429));
#8279=CARTESIAN_POINT('Ctrl Pts',(6.7778910457933,-5.99999999999995,15.2614647616422));
#8280=CARTESIAN_POINT('Ctrl Pts',(6.42385919064368,-5.99999999999994,15.6314481148128));
#8281=CARTESIAN_POINT('Ctrl Pts',(6.25585405294365,-5.99999999999994,15.8960743911704));
#8282=CARTESIAN_POINT('Ctrl Pts',(6.06020384677459,-5.99999999999994,16.3874179356908));
#8283=CARTESIAN_POINT('Ctrl Pts',(6.,-5.99999999999994,16.7029092618309));
#8284=CARTESIAN_POINT('Ctrl Pts',(6.,-5.99999999999994,16.9705627484772));
#8285=CARTESIAN_POINT('Origin',(0.,0.,0.));
#8286=CARTESIAN_POINT('Origin',(0.,-9.67470971326409E-15,-79.));
#8287=CARTESIAN_POINT('',(-5.49536666714402E-12,8.23880597151339,-68.5063651759543));
#8288=CARTESIAN_POINT('Ctrl Pts',(-5.99999895840801,8.18443806084714,-70.5266960994107));
#8289=CARTESIAN_POINT('Ctrl Pts',(-5.5690974342769,8.19291945646374,-70.200366972074));
#8290=CARTESIAN_POINT('Ctrl Pts',(-4.888010383118,8.20441278535078,-69.7661879460741));
#8291=CARTESIAN_POINT('Ctrl Pts',(-3.91204062649165,8.21698677095021,-69.2997698993554));
#8292=CARTESIAN_POINT('Ctrl Pts',(-3.16398253652809,8.22477080505801,-69.0142043719821));
#8293=CARTESIAN_POINT('Ctrl Pts',(-2.39663090139138,8.23094125189423,-68.7898200788163));
#8294=CARTESIAN_POINT('Ctrl Pts',(-1.61154890932236,8.23544005858267,-68.6273289139882));
#8295=CARTESIAN_POINT('Ctrl Pts',(-0.805544548123699,8.23819902126916,-68.5281353971799));
#8296=CARTESIAN_POINT('Ctrl Pts',(-0.268787035330602,8.23880659200157,-68.5063433790642));
#8297=CARTESIAN_POINT('Ctrl Pts',(-3.18401114664506E-12,8.23880597151339,
-68.5063651759543));
#8298=CARTESIAN_POINT('',(-2.73500395030388E-10,68.5063670000441,-8.2388058234896));
#8299=CARTESIAN_POINT('Origin',(1.22464679914735E-15,0.,0.));
#8300=CARTESIAN_POINT('',(-5.99999715845766,70.5267006388891,-8.18443795663603));
#8301=CARTESIAN_POINT('Ctrl Pts',(-2.73511885838946E-10,68.5063670000441,
-8.23880582348961));
#8302=CARTESIAN_POINT('Ctrl Pts',(-0.00373884108269842,68.5063664082688,
-8.2388058387049));
#8303=CARTESIAN_POINT('Ctrl Pts',(-0.00747734760339464,68.5063679389705,
-8.23880579472993));
#8304=CARTESIAN_POINT('Ctrl Pts',(-0.0112155109279515,68.5063715920789,
-8.23880569156401));
#8305=CARTESIAN_POINT('Ctrl Pts',(-0.0121232949516723,68.506372479208,-8.23880566651096));
#8306=CARTESIAN_POINT('Ctrl Pts',(-0.0130310587363146,68.5063734915004,
-8.23880563796729));
#8307=CARTESIAN_POINT('Ctrl Pts',(-0.0139388023081085,68.506374628946,-8.23880560593331));
#8308=CARTESIAN_POINT('Ctrl Pts',(-0.282917995094099,68.5067116725797,-8.23879611374476));
#8309=CARTESIAN_POINT('Ctrl Pts',(-0.550108573868126,68.518036776789,-8.2384805240124));
#8310=CARTESIAN_POINT('Ctrl Pts',(-0.81624500940925,68.5400862637072,-8.23786687734688));
#8311=CARTESIAN_POINT('Ctrl Pts',(-0.818721129250123,68.5402914110104,-8.23786116800956));
#8312=CARTESIAN_POINT('Ctrl Pts',(-0.821197157164274,68.5404974866639,-8.2378554328535));
#8313=CARTESIAN_POINT('Ctrl Pts',(-0.823673093694567,68.5407044904533,-8.23784967188635));
#8314=CARTESIAN_POINT('Ctrl Pts',(-1.08731389025658,68.562746511014,-8.23723623694985));
#8315=CARTESIAN_POINT('Ctrl Pts',(-1.34991844716521,68.595312828994,-8.23633012591871));
#8316=CARTESIAN_POINT('Ctrl Pts',(-1.61124780956339,68.6384063740778,-8.23513519709042));
#8317=CARTESIAN_POINT('Ctrl Pts',(-1.61706443909913,68.6393655437051,-8.23510860054477));
#8318=CARTESIAN_POINT('Ctrl Pts',(-1.6228804407311,68.6403299288959,-8.2350818604792));
#8319=CARTESIAN_POINT('Ctrl Pts',(-1.62869581330632,68.6412995298965,-8.23505497690792));
#8320=CARTESIAN_POINT('Ctrl Pts',(-1.88660702918973,68.6843012412662,-8.23386269310027));
#8321=CARTESIAN_POINT('Ctrl Pts',(-2.14328123564365,68.7375593459786,-8.2323882178511));
#8322=CARTESIAN_POINT('Ctrl Pts',(-2.39893596892781,68.8014424014476,-8.23062526198179));
#8323=CARTESIAN_POINT('Ctrl Pts',(-2.40804734805945,68.8037191546725,-8.23056243130735));
#8324=CARTESIAN_POINT('Ctrl Pts',(-2.41715726285983,68.8060093642543,-8.23049923764878));
#8325=CARTESIAN_POINT('Ctrl Pts',(-2.42626571371847,68.8083130436881,-8.23043568090945));
#8326=CARTESIAN_POINT('Ctrl Pts',(-2.67849247305856,68.8721054060963,-8.22867569881752));
#8327=CARTESIAN_POINT('Ctrl Pts',(-2.92959437693503,68.9462290809758,-8.22663723937388));
#8328=CARTESIAN_POINT('Ctrl Pts',(-3.17579288399155,69.0294813142028,-8.22436060167555));
#8329=CARTESIAN_POINT('Ctrl Pts',(-3.18802172175186,69.0336165060262,-8.22424751962081));
#8330=CARTESIAN_POINT('Ctrl Pts',(-3.2002384390651,69.0377742047295,-8.22413384470118));
#8331=CARTESIAN_POINT('Ctrl Pts',(-3.21244258772405,69.0419542652417,-8.22401958158434));
#8332=CARTESIAN_POINT('Ctrl Pts',(-3.47069841243532,69.1304098392505,-8.2216016238637));
#8333=CARTESIAN_POINT('Ctrl Pts',(-3.72332652714384,69.2288791839828,-8.21892027353038));
#8334=CARTESIAN_POINT('Ctrl Pts',(-3.97115318499118,69.3372405923039,-8.21598633637045));
#8335=CARTESIAN_POINT('Ctrl Pts',(-4.20020274943883,69.4373917769846,-8.21327469495772));
#8336=CARTESIAN_POINT('Ctrl Pts',(-4.42515017140143,69.545992763761,-8.21034729396852));
#8337=CARTESIAN_POINT('Ctrl Pts',(-4.64577000290152,69.6628850216051,-8.20721520875059));
#8338=CARTESIAN_POINT('Ctrl Pts',(-4.66424094621694,69.6726715863666,-8.20695298133374));
#8339=CARTESIAN_POINT('Ctrl Pts',(-4.68267694908691,69.6825138207613,-8.20668942620729));
#8340=CARTESIAN_POINT('Ctrl Pts',(-4.7010785817278,69.6924119031607,-8.20642454061931));
#8341=CARTESIAN_POINT('Ctrl Pts',(-4.83443960450597,69.764145668207,-8.2045048515558));
#8342=CARTESIAN_POINT('Ctrl Pts',(-4.96599736269102,69.83880901757,-8.20251537469265));
#8343=CARTESIAN_POINT('Ctrl Pts',(-5.09608337284685,69.9166283180189,-8.20045120283686));
#8344=CARTESIAN_POINT('Ctrl Pts',(-5.19900771676893,69.9781991236234,-8.19881802542029));
#8345=CARTESIAN_POINT('Ctrl Pts',(-5.30101022676462,70.0417463620704,-8.19713806766012));
#8346=CARTESIAN_POINT('Ctrl Pts',(-5.40224525221829,70.1074031078172,-8.19540839604894));
#8347=CARTESIAN_POINT('Ctrl Pts',(-5.52569971532715,70.1874704388553,-8.1932990897179));
#8348=CARTESIAN_POINT('Ctrl Pts',(-5.64801488356454,70.2706747960204,-8.19111584759849));
#8349=CARTESIAN_POINT('Ctrl Pts',(-5.76875558037752,70.356772821631,-8.18886619176866));
#8350=CARTESIAN_POINT('Ctrl Pts',(-5.84653233268286,70.4122340289011,-8.1874170455498));
#8351=CARTESIAN_POINT('Ctrl Pts',(-5.92365514224985,70.4688966414595,-8.18594032623917));
#8352=CARTESIAN_POINT('Ctrl Pts',(-5.99999716495239,70.5267006438067,-8.18443795650821));
#8353=CARTESIAN_POINT('',(-6.,70.5266968882281,8.18443804032995));
#8354=CARTESIAN_POINT('Origin',(-6.,-3.53369596958238E-16,0.));
#8355=CARTESIAN_POINT('',(-8.95159733014031E-12,68.5063647597673,8.23880598322944));
#8356=CARTESIAN_POINT('Ctrl Pts',(-5.99999948661478,70.5266964994307,8.18443805045074));
#8357=CARTESIAN_POINT('Ctrl Pts',(-5.78451154162507,70.3635037543157,8.18867948064694));
#8358=CARTESIAN_POINT('Ctrl Pts',(-5.34212806448152,70.055768219971,8.19674757400964));
#8359=CARTESIAN_POINT('Ctrl Pts',(-4.64059859463673,69.6477395339077,8.2076055215689));
#8360=CARTESIAN_POINT('Ctrl Pts',(-3.91292633842418,69.3002864631745,8.21697301436391));
#8361=CARTESIAN_POINT('Ctrl Pts',(-3.16585416162398,69.0148381621378,8.22475339508119));
#8362=CARTESIAN_POINT('Ctrl Pts',(-2.39835642218803,68.7901683634025,8.23093161161829));
#8363=CARTESIAN_POINT('Ctrl Pts',(-1.6087834219025,68.6267990516475,8.23545474346867));
#8364=CARTESIAN_POINT('Ctrl Pts',(-0.804180861593639,68.5281198274787,8.23819947080704));
#8365=CARTESIAN_POINT('Ctrl Pts',(-0.268573138561608,68.5063141973659,8.23880740764904));
#8366=CARTESIAN_POINT('Ctrl Pts',(-8.95159733014031E-12,68.5063647597673,
8.23880598322944));
#8367=CARTESIAN_POINT('',(-2.38940561989992E-10,8.23880549026604,68.5063639612443));
#8368=CARTESIAN_POINT('Origin',(1.22464679914735E-15,0.,0.));
#8369=CARTESIAN_POINT('Ctrl Pts',(-2.38940450967676E-10,8.23880549026604,
68.5063639612443));
#8370=CARTESIAN_POINT('Ctrl Pts',(-0.00119743047815034,8.23880548637175,
68.5063641815433));
#8371=CARTESIAN_POINT('Ctrl Pts',(-0.00239488142112834,8.2388054764133,
68.5063646198442));
#8372=CARTESIAN_POINT('Ctrl Pts',(-0.00359235313103486,8.23880546039038,
68.5063652761552));
#8373=CARTESIAN_POINT('Ctrl Pts',(-0.00477852616968188,8.23880544451865,
68.5063659262736));
#8374=CARTESIAN_POINT('Ctrl Pts',(-0.00596471919577684,8.23880542267338,
68.5063667903101));
#8375=CARTESIAN_POINT('Ctrl Pts',(-0.00715093227137261,8.23880539485422,
68.506367868272));
#8376=CARTESIAN_POINT('Ctrl Pts',(-0.275542599110005,8.23879910051263,68.5066117671079));
#8377=CARTESIAN_POINT('Ctrl Pts',(-0.544960513818001,8.23848697859665,68.5178073781331));
#8378=CARTESIAN_POINT('Ctrl Pts',(-0.811826492207112,8.23787592190724,68.5397251334166));
#8379=CARTESIAN_POINT('Ctrl Pts',(-0.817008824069481,8.23786405565674,68.5401507593515));
#8380=CARTESIAN_POINT('Ctrl Pts',(-0.822190223933388,8.23785207545356,68.540580431239));
#8381=CARTESIAN_POINT('Ctrl Pts',(-0.827370663690959,8.23783998143978,68.5410141473606));
#8382=CARTESIAN_POINT('Ctrl Pts',(-1.06376993820737,8.23728809468556,68.5608059374966));
#8383=CARTESIAN_POINT('Ctrl Pts',(-1.29816894019248,8.2364990940397,68.5890236262271));
#8384=CARTESIAN_POINT('Ctrl Pts',(-1.53073410795179,8.23548929589195,68.6254521884976));
#8385=CARTESIAN_POINT('Ctrl Pts',(-1.55667432227247,8.23537666346025,68.6295154139659));
#8386=CARTESIAN_POINT('Ctrl Pts',(-1.5825917325838,8.23526128548904,68.6336807394219));
#8387=CARTESIAN_POINT('Ctrl Pts',(-1.60848657744125,8.23514318567388,68.6379478275793));
#8388=CARTESIAN_POINT('Ctrl Pts',(-1.61754348689097,8.23510187940857,68.6394402725531));
#8389=CARTESIAN_POINT('Ctrl Pts',(-1.62659786881208,8.23506022841665,68.6409452057524));
#8390=CARTESIAN_POINT('Ctrl Pts',(-1.63564974610698,8.23501823312477,68.6424626167318));
#8391=CARTESIAN_POINT('Ctrl Pts',(-1.90269718744703,8.23377929286099,68.6872291006701));
#8392=CARTESIAN_POINT('Ctrl Pts',(-2.16756507620287,8.23224073153665,68.7428541162553));
#8393=CARTESIAN_POINT('Ctrl Pts',(-2.43002969761608,8.23040991820687,68.8092649879185));
#8394=CARTESIAN_POINT('Ctrl Pts',(-2.67563111594158,8.2286967335953,68.8714089987376));
#8395=CARTESIAN_POINT('Ctrl Pts',(-2.91912792037934,8.22672764247879,68.9429974373362));
#8396=CARTESIAN_POINT('Ctrl Pts',(-3.16108135489304,8.22449604172108,69.0244973202163));
#8397=CARTESIAN_POINT('Ctrl Pts',(-3.17757512971591,8.2243439152573,69.0300531029602));
#8398=CARTESIAN_POINT('Ctrl Pts',(-3.19405954559071,8.22419061910876,69.0356542108646));
#8399=CARTESIAN_POINT('Ctrl Pts',(-3.21053495270791,8.22403614735284,69.0413008166669));
#8400=CARTESIAN_POINT('Ctrl Pts',(-3.38604792150681,8.22239055545433,69.1014542648307));
#8401=CARTESIAN_POINT('Ctrl Pts',(-3.56053902191876,8.2206116630597,69.166766732304));
#8402=CARTESIAN_POINT('Ctrl Pts',(-3.7329361227573,8.21870979242949,69.2368236563124));
#8403=CARTESIAN_POINT('Ctrl Pts',(-3.79419891986031,8.21803394629305,69.2617189886603));
#8404=CARTESIAN_POINT('Ctrl Pts',(-3.85519719392959,8.21734255808504,69.2872139255654));
#8405=CARTESIAN_POINT('Ctrl Pts',(-3.9158822437057,8.21663605348593,69.3132913313463));
#8406=CARTESIAN_POINT('Ctrl Pts',(-3.93571269242953,8.21640518437932,69.3218128149752));
#8407=CARTESIAN_POINT('Ctrl Pts',(-3.95551155625911,8.21617269798135,69.3303973027179));
#8408=CARTESIAN_POINT('Ctrl Pts',(-3.97527663721697,8.21593862172726,69.3390440387009));
#8409=CARTESIAN_POINT('Ctrl Pts',(-4.18546974883883,8.21344932171843,69.4309983466808));
#8410=CARTESIAN_POINT('Ctrl Pts',(-4.39183988326306,8.21078011928237,69.5299962380484));
#8411=CARTESIAN_POINT('Ctrl Pts',(-4.59434450063668,8.20794530577172,69.6358149303183));
#8412=CARTESIAN_POINT('Ctrl Pts',(-4.61044583130454,8.20771990711015,69.6442286730624));
#8413=CARTESIAN_POINT('Ctrl Pts',(-4.62652273854098,8.20749346207156,69.6526855137308));
#8414=CARTESIAN_POINT('Ctrl Pts',(-4.6425752083125,8.20726597815253,69.6611853284648));
#8415=CARTESIAN_POINT('Ctrl Pts',(-4.6646451753276,8.20695321864193,69.6728714199812));
#8416=CARTESIAN_POINT('Ctrl Pts',(-4.68666871769243,8.20663846427466,69.6846386242432));
#8417=CARTESIAN_POINT('Ctrl Pts',(-4.70864603612887,8.20632172869146,69.6964867360917));
#8418=CARTESIAN_POINT('Ctrl Pts',(-5.02435114272387,8.20177180867526,69.8666853626846));
#8419=CARTESIAN_POINT('Ctrl Pts',(-5.33051997376249,8.19681310827977,70.0535759591058));
#8420=CARTESIAN_POINT('Ctrl Pts',(-5.62708060760958,8.19146556534272,70.2574709713756));
#8421=CARTESIAN_POINT('Ctrl Pts',(-5.75312566204789,8.18919273724726,70.3441310165336));
#8422=CARTESIAN_POINT('Ctrl Pts',(-5.87743471628307,8.18684965924949,70.4338633607541));
#8423=CARTESIAN_POINT('Ctrl Pts',(-6.00000075752689,8.18443783045391,70.5266944330751));
#8424=CARTESIAN_POINT('',(4.16525128190542E-10,-8.23880590935122,68.5063673993547));
#8425=CARTESIAN_POINT('Ctrl Pts',(-5.99999999999998,-8.18443804034557,70.5266968882263));
#8426=CARTESIAN_POINT('Ctrl Pts',(-5.78418052149934,-8.18868599659508,70.3632530453486));
#8427=CARTESIAN_POINT('Ctrl Pts',(-5.33854958945116,-8.19680831145233,70.0534670788763));
#8428=CARTESIAN_POINT('Ctrl Pts',(-4.41053460175808,-8.21115661661037,69.5143250649606));
#8429=CARTESIAN_POINT('Ctrl Pts',(-3.43120662489604,-8.22261256046406,69.0927024818813));
#8430=CARTESIAN_POINT('Ctrl Pts',(-2.39407107542595,-8.23096914645052,68.7888010655747));
#8431=CARTESIAN_POINT('Ctrl Pts',(-1.60026509897427,-8.23549084886545,68.6255002091326));
#8432=CARTESIAN_POINT('Ctrl Pts',(-0.80294392845351,-8.23820151213957,68.5280473459781));
#8433=CARTESIAN_POINT('Ctrl Pts',(-0.265147204082705,-8.23880460260968,
68.5064140674028));
#8434=CARTESIAN_POINT('Ctrl Pts',(4.16541472538293E-10,-8.23880590935122,
68.5063673993548));
#8435=CARTESIAN_POINT('',(-3.51061826131195E-10,-68.5063672600388,8.23880581768755));
#8436=CARTESIAN_POINT('Origin',(1.22464679914735E-15,0.,0.));
#8437=CARTESIAN_POINT('Ctrl Pts',(-3.51073400206478E-10,-68.5063672600388,
8.23880581768755));
#8438=CARTESIAN_POINT('Ctrl Pts',(-0.00385818621438253,-68.5063665769295,
8.23880583540891));
#8439=CARTESIAN_POINT('Ctrl Pts',(-0.00771604492353719,-68.5063681582155,
8.23880578998357));
#8440=CARTESIAN_POINT('Ctrl Pts',(-0.0115735656074801,-68.5063720042282,
8.23880568139922));
#8441=CARTESIAN_POINT('Ctrl Pts',(-0.0116031125215163,-68.506372033687,
8.23880568056751));
#8442=CARTESIAN_POINT('Ctrl Pts',(-0.0116326594157389,-68.5063720632786,
8.2388056797321));
#8443=CARTESIAN_POINT('Ctrl Pts',(-0.0116622062901124,-68.5063720930031,
8.23880567889298));
#8444=CARTESIAN_POINT('Ctrl Pts',(-0.28104379280587,-68.5066430940673,8.23879802856396));
#8445=CARTESIAN_POINT('Ctrl Pts',(-0.548776288907163,-68.5179577377854,
8.23848251126927));
#8446=CARTESIAN_POINT('Ctrl Pts',(-0.815115448555507,-68.5399926087912,
8.23786943479957));
#8447=CARTESIAN_POINT('Ctrl Pts',(-0.818638638156674,-68.5402840906314,
8.23786132489698));
#8448=CARTESIAN_POINT('Ctrl Pts',(-0.822161582922775,-68.540577448376,8.23785316286225));
#8449=CARTESIAN_POINT('Ctrl Pts',(-0.825684283357457,-68.5408726812731,
8.23784494871921));
#8450=CARTESIAN_POINT('Ctrl Pts',(-1.08846376352508,-68.5628958844056,8.23723220622846));
#8451=CARTESIAN_POINT('Ctrl Pts',(-1.34988356665061,-68.5953539573717,8.23632949102674));
#8452=CARTESIAN_POINT('Ctrl Pts',(-1.60969559173261,-68.6381510212431,8.2351425283051));
#8453=CARTESIAN_POINT('Ctrl Pts',(-1.61671526827113,-68.6393073247093,8.23511045860252));
#8454=CARTESIAN_POINT('Ctrl Pts',(-1.62373379075566,-68.6404711784755,8.2350781807139));
#8455=CARTESIAN_POINT('Ctrl Pts',(-1.63075115562209,-68.6416425809445,8.23504569477409));
#8456=CARTESIAN_POINT('Ctrl Pts',(-1.88694202943979,-68.6844082954009,8.23385969383694));
#8457=CARTESIAN_POINT('Ctrl Pts',(-2.14159007557437,-68.7372339187662,8.2323964294449));
#8458=CARTESIAN_POINT('Ctrl Pts',(-2.39544154112822,-68.8005695892671,8.23064983883997));
#8459=CARTESIAN_POINT('Ctrl Pts',(-2.40589777583131,-68.8031784086978,8.2305778961342));
#8460=CARTESIAN_POINT('Ctrl Pts',(-2.41635237751087,-68.8058049920654,8.23050547446862));
#8461=CARTESIAN_POINT('Ctrl Pts',(-2.42680539922861,-68.8084493687539,8.23043257324636));
#8462=CARTESIAN_POINT('Ctrl Pts',(-2.67707698890509,-68.8717623872676,8.22868713491521));
#8463=CARTESIAN_POINT('Ctrl Pts',(-2.92644200671099,-68.9452735301382,8.22666684341862));
#8464=CARTESIAN_POINT('Ctrl Pts',(-3.17155833115999,-69.0280482116615,8.22440186183105));
#8465=CARTESIAN_POINT('Ctrl Pts',(-3.18529986316834,-69.0326886652836,8.22427488409078));
#8466=CARTESIAN_POINT('Ctrl Pts',(-3.19902855252207,-69.0373584099793,8.22414713390775));
#8467=CARTESIAN_POINT('Ctrl Pts',(-3.21274375596388,-69.0420572713038,8.22401861745451));
#8468=CARTESIAN_POINT('Ctrl Pts',(-3.43326552071907,-69.1176085524791,8.22195224817393));
#8469=CARTESIAN_POINT('Ctrl Pts',(-3.65029895515285,-69.2006910611612,8.21968767912429));
#8470=CARTESIAN_POINT('Ctrl Pts',(-3.86355207639196,-69.2909505112194,8.21724088229277));
#8471=CARTESIAN_POINT('Ctrl Pts',(-3.88349996596054,-69.2993934616991,8.21701200670723));
#8472=CARTESIAN_POINT('Ctrl Pts',(-3.90341479510208,-69.3078991761863,8.21678153750259));
#8473=CARTESIAN_POINT('Ctrl Pts',(-3.92329633543422,-69.316467344228,8.21654948826908));
#8474=CARTESIAN_POINT('Ctrl Pts',(-3.93993217901766,-69.3236367436286,8.21635532148483));
#8475=CARTESIAN_POINT('Ctrl Pts',(-3.9565447498138,-69.3308498856566,8.21616003519082));
#8476=CARTESIAN_POINT('Ctrl Pts',(-3.97313405731919,-69.338106650427,8.2159636358534));
#8477=CARTESIAN_POINT('Ctrl Pts',(-4.20150197396974,-69.4380030597072,8.21326000838113));
#8478=CARTESIAN_POINT('Ctrl Pts',(-4.42546345991262,-69.546162167036,8.21034555688662));
#8479=CARTESIAN_POINT('Ctrl Pts',(-4.64518491558962,-69.6625713356289,8.20722979971519));
#8480=CARTESIAN_POINT('Ctrl Pts',(-4.66456114572406,-69.6728369277326,8.20695503534223));
#8481=CARTESIAN_POINT('Ctrl Pts',(-4.68390071403998,-69.6831647622597,8.20667874858075));
#8482=CARTESIAN_POINT('Ctrl Pts',(-4.70320400447882,-69.6935549071169,8.20640094242959));
#8483=CARTESIAN_POINT('Ctrl Pts',(-4.86547624806854,-69.7808991929293,8.20406557750431));
#8484=CARTESIAN_POINT('Ctrl Pts',(-5.02518681123594,-69.8726431417192,8.20162293160604));
#8485=CARTESIAN_POINT('Ctrl Pts',(-5.18266532395224,-69.9690359345141,8.19906977102499));
#8486=CARTESIAN_POINT('Ctrl Pts',(-5.25664466501042,-70.0143187808576,8.19787036207616));
#8487=CARTESIAN_POINT('Ctrl Pts',(-5.33013106871451,-70.0606282200054,8.1966465478237));
#8488=CARTESIAN_POINT('Ctrl Pts',(-5.40315693610489,-70.1079936559069,8.19539790722249));
#8489=CARTESIAN_POINT('Ctrl Pts',(-5.55655477109986,-70.2074892946516,8.19277501794013));
#8490=CARTESIAN_POINT('Ctrl Pts',(-5.70792279166802,-70.3116421098362,8.19004263268351));
#8491=CARTESIAN_POINT('Ctrl Pts',(-5.85676761348635,-70.4202342062778,8.18721006457127));
#8492=CARTESIAN_POINT('Ctrl Pts',(-5.90477990751254,-70.4552623355709,8.18629637411572));
#8493=CARTESIAN_POINT('Ctrl Pts',(-5.95252939627508,-70.4907526632035,8.18537225351234));
#8494=CARTESIAN_POINT('Ctrl Pts',(-5.99999865521153,-70.5266986694858,8.18443799940374));
#8495=CARTESIAN_POINT('',(-1.22464679914735E-15,-68.5063652081765,-8.2388061006397));
#8496=CARTESIAN_POINT('Ctrl Pts',(-5.99999923045746,-70.5266963054383,-8.18443805549265));
#8497=CARTESIAN_POINT('Ctrl Pts',(-5.87027903212654,-70.4284569638484,-8.18699132655943));
#8498=CARTESIAN_POINT('Ctrl Pts',(-5.73842754629939,-70.3335701958321,-8.18947252824115));
#8499=CARTESIAN_POINT('Ctrl Pts',(-5.60435418714887,-70.2419484360896,-8.19187705488044));
#8500=CARTESIAN_POINT('Ctrl Pts',(-5.51565628121315,-70.1813349161569,-8.1934677995222));
#8501=CARTESIAN_POINT('Ctrl Pts',(-5.42598523691919,-70.122151187232,-8.19502506306265));
#8502=CARTESIAN_POINT('Ctrl Pts',(-5.3353077250708,-70.0643821800456,-8.19654852892693));
#8503=CARTESIAN_POINT('Ctrl Pts',(-5.2178641440315,-69.9895609929755,-8.19852168944981));
#8504=CARTESIAN_POINT('Ctrl Pts',(-5.09872782901844,-69.9171169607333,-8.20043878610134));
#8505=CARTESIAN_POINT('Ctrl Pts',(-4.97824262075468,-69.8472641180671,-8.20229660945547));
#8506=CARTESIAN_POINT('Ctrl Pts',(-4.865086125733,-69.7816601907692,-8.20404142761325));
#8507=CARTESIAN_POINT('Ctrl Pts',(-4.75074030582435,-69.7183415425653,-8.20573394692875));
#8508=CARTESIAN_POINT('Ctrl Pts',(-4.63551013050863,-69.6574489672838,-8.20736745994599));
#8509=CARTESIAN_POINT('Ctrl Pts',(-4.46498601115885,-69.5673366963759,-8.20978482473736));
#8510=CARTESIAN_POINT('Ctrl Pts',(-4.2925273749644,-69.4825256560631,-8.21207037874011));
#8511=CARTESIAN_POINT('Ctrl Pts',(-4.11819334568071,-69.4029361694811,-8.21422081851545));
#8512=CARTESIAN_POINT('Ctrl Pts',(-3.94271063860926,-69.3228222719408,-8.21638542742584));
#8513=CARTESIAN_POINT('Ctrl Pts',(-3.76532722073528,-69.2479986650071,-8.21841309567276));
#8514=CARTESIAN_POINT('Ctrl Pts',(-3.58607414262684,-69.1784279779047,-8.22030371422339));
#8515=CARTESIAN_POINT('Ctrl Pts',(-3.44647633668207,-69.1242480699218,-8.22177608058012));
#8516=CARTESIAN_POINT('Ctrl Pts',(-3.30574393103558,-69.073254855566,-8.22316538895211));
#8517=CARTESIAN_POINT('Ctrl Pts',(-3.16388256600053,-69.0254505692774,-8.22447316069163));
#8518=CARTESIAN_POINT('Ctrl Pts',(-3.01568852837794,-68.9755123059664,-8.22583931118877));
#8519=CARTESIAN_POINT('Ctrl Pts',(-2.86626984965028,-68.9290537059868,-8.22711708905403));
#8520=CARTESIAN_POINT('Ctrl Pts',(-2.71547697134612,-68.8860638985536,-8.22829946064218));
#8521=CARTESIAN_POINT('Ctrl Pts',(-2.60934779248849,-68.855807343911,-8.2291316227918));
#8522=CARTESIAN_POINT('Ctrl Pts',(-2.50253757802254,-68.8272700577375,-8.22991663042879));
#8523=CARTESIAN_POINT('Ctrl Pts',(-2.39499130075912,-68.8004633954027,-8.23065360525647));
#8524=CARTESIAN_POINT('Ctrl Pts',(-2.26395851548226,-68.7678025565611,-8.23155152442956));
#8525=CARTESIAN_POINT('Ctrl Pts',(-2.13182992580535,-68.7377160415585,-8.23237878926188));
#8526=CARTESIAN_POINT('Ctrl Pts',(-1.9989917728853,-68.7103301969358,-8.23313611364337));
#8527=CARTESIAN_POINT('Ctrl Pts',(-1.86789016177572,-68.683302356871,-8.23388353781604));
#8528=CARTESIAN_POINT('Ctrl Pts',(-1.73609775085767,-68.6589050200765,-8.23456284263883));
#8529=CARTESIAN_POINT('Ctrl Pts',(-1.60399728261137,-68.6372115535411,-8.23516858331626));
#8530=CARTESIAN_POINT('Ctrl Pts',(-1.38764322858426,-68.6016820093,-8.23616066497192));
#8531=CARTESIAN_POINT('Ctrl Pts',(-1.17046576101213,-68.5733904177854,-8.23695222102039));
#8532=CARTESIAN_POINT('Ctrl Pts',(-0.952624108263045,-68.5523229098841,
-8.23753982863067));
#8533=CARTESIAN_POINT('Ctrl Pts',(-0.734950166798859,-68.5312716213733,
-8.23812698385535));
#8534=CARTESIAN_POINT('Ctrl Pts',(-0.516612293295068,-68.5174332298595,
-8.23851049823526));
#8535=CARTESIAN_POINT('Ctrl Pts',(-0.297763899889859,-68.5108453651861,
-8.23868919922455));
#8536=CARTESIAN_POINT('Ctrl Pts',(-0.198609217040279,-68.5078605699944,
-8.23877016413201));
#8537=CARTESIAN_POINT('Ctrl Pts',(-0.0993497327048553,-68.5063648454567,
-8.23880911668573));
#8538=CARTESIAN_POINT('Ctrl Pts',(-1.22464679914735E-15,-68.5063652081765,
-8.23880610063971));
#8539=CARTESIAN_POINT('',(-7.6571373978539E-15,-8.23880518655814,-68.5063653181071));
#8540=CARTESIAN_POINT('Origin',(1.22464679914735E-15,0.,0.));
#8541=CARTESIAN_POINT('Ctrl Pts',(-7.6571373978539E-15,-8.23880518655807,
-68.5063653181071));
#8542=CARTESIAN_POINT('Ctrl Pts',(-0.00206351045186059,-8.23880544768633,
-68.5063652867029));
#8543=CARTESIAN_POINT('Ctrl Pts',(-0.00412693915927323,-8.23880569090796,
-68.506365900766));
#8544=CARTESIAN_POINT('Ctrl Pts',(-0.0061902852373708,-8.2388059161998,
-68.5063671601456));
#8545=CARTESIAN_POINT('Ctrl Pts',(-0.168945921413918,-8.23882368709946,
-68.5064664993328));
#8546=CARTESIAN_POINT('Ctrl Pts',(-0.331181753910835,-8.23872945968339,
-68.5105766381394));
#8547=CARTESIAN_POINT('Ctrl Pts',(-0.493021483442529,-8.23851680360619,
-68.5186485086519));
#8548=CARTESIAN_POINT('Ctrl Pts',(-0.655074028978294,-8.23830386789052,
-68.5267309935124));
#8549=CARTESIAN_POINT('Ctrl Pts',(-0.816729897949388,-8.23797219477017,
-68.5387856576554));
#8550=CARTESIAN_POINT('Ctrl Pts',(-0.978113579330973,-8.23752036276245,
-68.5548152559583));
#8551=CARTESIAN_POINT('Ctrl Pts',(-1.13917076696477,-8.23706944485165,-68.5708124249375));
#8552=CARTESIAN_POINT('Ctrl Pts',(-1.29995732955209,-8.23649886288153,-68.5907685178097));
#8553=CARTESIAN_POINT('Ctrl Pts',(-1.46059033272571,-8.23581211997273,-68.614737415174));
#8554=CARTESIAN_POINT('Ctrl Pts',(-1.50766644276116,-8.23561085881157,-68.6217618897679));
#8555=CARTESIAN_POINT('Ctrl Pts',(-1.55472929520138,-8.2353996525357,-68.6291313474598));
#8556=CARTESIAN_POINT('Ctrl Pts',(-1.60178163876484,-8.23517866757182,-68.6368479678193));
#8557=CARTESIAN_POINT('Ctrl Pts',(-1.74949257113952,-8.23448493177496,-68.6610726737907));
#8558=CARTESIAN_POINT('Ctrl Pts',(-1.89710107729826,-8.23369575365773,-68.6887235288312));
#8559=CARTESIAN_POINT('Ctrl Pts',(-2.04420312931326,-8.23282291319157,-68.7197671066736));
#8560=CARTESIAN_POINT('Ctrl Pts',(-2.19121197202044,-8.23195062578946,-68.7507910141554));
#8561=CARTESIAN_POINT('Ctrl Pts',(-2.33771464560452,-8.23099476748653,-68.7852032984919));
#8562=CARTESIAN_POINT('Ctrl Pts',(-2.48331624371162,-8.22996030290718,-68.822919674804));
#8563=CARTESIAN_POINT('Ctrl Pts',(-2.62904439646648,-8.22892493918728,-68.8606688336046));
#8564=CARTESIAN_POINT('Ctrl Pts',(-2.7738695573344,-8.22781081116615,-68.901727740215));
#8565=CARTESIAN_POINT('Ctrl Pts',(-2.91740947016524,-8.22661635650124,-68.9459618822334));
#8566=CARTESIAN_POINT('Ctrl Pts',(-3.00103310871868,-8.22592048980328,-68.9717318568064));
#8567=CARTESIAN_POINT('Ctrl Pts',(-3.08422081663934,-8.2251972393183,-68.9985785790516));
#8568=CARTESIAN_POINT('Ctrl Pts',(-3.16689985036813,-8.22444532483442,-69.0264678697792));
#8569=CARTESIAN_POINT('Ctrl Pts',(-3.32589426532498,-8.22299936933555,-69.0800998640443));
#8570=CARTESIAN_POINT('Ctrl Pts',(-3.48301497421291,-8.22144690169077,-69.1375833051657));
#8571=CARTESIAN_POINT('Ctrl Pts',(-3.63837777161623,-8.21978673379442,-69.1988932866378));
#8572=CARTESIAN_POINT('Ctrl Pts',(-3.79404440644263,-8.21812331916755,-69.2603231698309));
#8573=CARTESIAN_POINT('Ctrl Pts',(-3.94794670471723,-8.21635180738967,-69.325594744792));
#8574=CARTESIAN_POINT('Ctrl Pts',(-4.10018577887777,-8.21447595386902,-69.3947327342989));
#8575=CARTESIAN_POINT('Ctrl Pts',(-4.25226186536004,-8.21260210864363,-69.4637967044356));
#8576=CARTESIAN_POINT('Ctrl Pts',(-4.40267872776132,-8.2106241749733,-69.5367190183991));
#8577=CARTESIAN_POINT('Ctrl Pts',(-4.5515151235918,-8.20855041683867,-69.6135711035785));
#8578=CARTESIAN_POINT('Ctrl Pts',(-4.58036246705801,-8.20814848280337,-69.628466509268));
#8579=CARTESIAN_POINT('Ctrl Pts',(-4.6091503609389,-8.20774296187061,-69.6435096758942));
#8580=CARTESIAN_POINT('Ctrl Pts',(-4.6378792610473,-8.20733393235838,-69.6587013169032));
#8581=CARTESIAN_POINT('Ctrl Pts',(-4.80509780639098,-8.20495314785988,-69.7471253116028));
#8582=CARTESIAN_POINT('Ctrl Pts',(-4.97030250657127,-8.20245399782115,-69.8405765183875));
#8583=CARTESIAN_POINT('Ctrl Pts',(-5.13305779370999,-8.1998458336701,-69.9388954647287));
#8584=CARTESIAN_POINT('Ctrl Pts',(-5.29568134156507,-8.19723978064971,-70.0371348286011));
#8585=CARTESIAN_POINT('Ctrl Pts',(-5.45585907554819,-8.19452484502024,-70.1402339115534));
#8586=CARTESIAN_POINT('Ctrl Pts',(-5.61317670591776,-8.19170441954395,-70.2479860613005));
#8587=CARTESIAN_POINT('Ctrl Pts',(-5.74417600481268,-8.18935583496947,-70.3377118983739));
#8588=CARTESIAN_POINT('Ctrl Pts',(-5.87319237329383,-8.1869339839657,-70.4306632680959));
#8589=CARTESIAN_POINT('Ctrl Pts',(-6.00000000000001,-8.18443804034608,-70.5266968882262));
#8590=CARTESIAN_POINT('Ctrl Pts',(6.,-8.18443804034608,-70.5266968882262));
#8591=CARTESIAN_POINT('Ctrl Pts',(5.83935589890228,-8.1875999843835,-70.4050383178254));
#8592=CARTESIAN_POINT('Ctrl Pts',(5.67578673642156,-8.19064303069535,-70.2887847010274));
#8593=CARTESIAN_POINT('Ctrl Pts',(5.50942106147531,-8.19356119742072,-70.1778680148472));
#8594=CARTESIAN_POINT('Ctrl Pts',(5.34128427556694,-8.19651043063309,-70.0657705216355));
#8595=CARTESIAN_POINT('Ctrl Pts',(5.17029064779969,-8.19933205929434,-69.9591237634446));
#8596=CARTESIAN_POINT('Ctrl Pts',(4.99653358519068,-8.20202243644602,-69.8578934495407));
#8597=CARTESIAN_POINT('Ctrl Pts',(4.8804127072399,-8.20382040052403,-69.7902417941246));
#8598=CARTESIAN_POINT('Ctrl Pts',(4.76305682585017,-8.20555979931183,-69.7250099731657));
#8599=CARTESIAN_POINT('Ctrl Pts',(4.64448583892399,-8.20724032943103,-69.6621979344201));
#8600=CARTESIAN_POINT('Ctrl Pts',(4.48748709677556,-8.2094655037481,-69.5790290975023));
#8601=CARTESIAN_POINT('Ctrl Pts',(4.32836434918063,-8.21158809145558,-69.5001027126829));
#8602=CARTESIAN_POINT('Ctrl Pts',(4.16706106631021,-8.21360403193805,-69.4254068252458));
#8603=CARTESIAN_POINT('Ctrl Pts',(4.08612566398949,-8.21461554857367,-69.3879274783048));
#8604=CARTESIAN_POINT('Ctrl Pts',(4.00464093265679,-8.21560028549895,-69.351513944954));
#8605=CARTESIAN_POINT('Ctrl Pts',(3.92259791175199,-8.21655817297074,-69.3161692970076));
#8606=CARTESIAN_POINT('Ctrl Pts',(3.72085798171443,-8.21891357321577,-69.2292584699165));
#8607=CARTESIAN_POINT('Ctrl Pts',(3.515745117614,-8.22110667449109,-69.1488092724985));
#8608=CARTESIAN_POINT('Ctrl Pts',(3.30737505839146,-8.22311989481481,-69.0750285052789));
#8609=CARTESIAN_POINT('Ctrl Pts',(3.26212128379759,-8.22355712566783,-69.0590048106004));
#8610=CARTESIAN_POINT('Ctrl Pts',(3.21671388216392,-8.22398588824251,-69.0432958404281));
#8611=CARTESIAN_POINT('Ctrl Pts',(3.17115406088249,-8.22440602934023,-69.0279040399477));
#8612=CARTESIAN_POINT('Ctrl Pts',(3.04348452784257,-8.22558336534041,-68.9847725279113));
#8613=CARTESIAN_POINT('Ctrl Pts',(2.91461436345215,-8.22669344285102,-68.9441351923562));
#8614=CARTESIAN_POINT('Ctrl Pts',(2.784937514944,-8.2277368326506,-68.9061417077793));
#8615=CARTESIAN_POINT('Ctrl Pts',(2.65526066643585,-8.22878022245018,-68.8681482232025));
#8616=CARTESIAN_POINT('Ctrl Pts',(2.52477746828391,-8.22975694690195,-68.8327986930296));
#8617=CARTESIAN_POINT('Ctrl Pts',(2.39389751143945,-8.23066112223301,-68.8001908239837));
#8618=CARTESIAN_POINT('Ctrl Pts',(2.24586149903464,-8.23168381901373,-68.7633086380252));
#8619=CARTESIAN_POINT('Ctrl Pts',(2.09732185681607,-8.23261249774906,-68.7299245554918));
#8620=CARTESIAN_POINT('Ctrl Pts',(1.94812127075837,-8.23344107483214,-68.6999793435983));
#8621=CARTESIAN_POINT('Ctrl Pts',(1.83350272325276,-8.23407760250451,-68.6769748984907));
#8622=CARTESIAN_POINT('Ctrl Pts',(1.71849372454123,-8.23465515294992,-68.6560009217279));
#8623=CARTESIAN_POINT('Ctrl Pts',(1.6030186314804,-8.2351730392858,-68.6370508939283));
#8624=CARTESIAN_POINT('Ctrl Pts',(1.44517413123055,-8.23588094527407,-68.6111478390924));
#8625=CARTESIAN_POINT('Ctrl Pts',(1.28644990400479,-8.23647732620875,-68.589032311698));
#8626=CARTESIAN_POINT('Ctrl Pts',(1.12724839634008,-8.23697240718817,-68.5707819182047));
#8627=CARTESIAN_POINT('Ctrl Pts',(0.96806767754036,-8.23746742351888,-68.5525339078858));
#8628=CARTESIAN_POINT('Ctrl Pts',(0.808410173874957,-8.23786117621294,-68.5381500692541));
#8629=CARTESIAN_POINT('Ctrl Pts',(0.648684626042312,-8.23815664722233,-68.5276567709296));
#8630=CARTESIAN_POINT('Ctrl Pts',(0.488781786876221,-8.2384524461971,-68.5171518253084));
#8631=CARTESIAN_POINT('Ctrl Pts',(0.328811127110583,-8.23864974756345,-68.5105460654646));
#8632=CARTESIAN_POINT('Ctrl Pts',(0.169183612391038,-8.23874419313204,-68.5078142233184));
#8633=CARTESIAN_POINT('Ctrl Pts',(0.112740170955557,-8.2387775885835,-68.5068482584441));
#8634=CARTESIAN_POINT('Ctrl Pts',(0.0563396137314528,-8.23879805702532,
-68.5063661755286));
#8635=CARTESIAN_POINT('Ctrl Pts',(-7.6571373978539E-15,-8.23880518655807,
-68.5063653181071));
#8636=CARTESIAN_POINT('Ctrl Pts',(-1.22464679914735E-15,-68.5063652081765,
-8.23880610063971));
#8637=CARTESIAN_POINT('Ctrl Pts',(0.00143095575713891,-68.5063652134009,
-8.23880605719895));
#8638=CARTESIAN_POINT('Ctrl Pts',(0.00286193022978105,-68.5063655290304,
-8.23880600505331));
#8639=CARTESIAN_POINT('Ctrl Pts',(0.00429292337380016,-68.5063661550895,
-8.23880594420307));
#8640=CARTESIAN_POINT('Ctrl Pts',(0.139173304405083,-68.5064251652143,-8.23880020867207));
#8641=CARTESIAN_POINT('Ctrl Pts',(0.274219837871558,-68.5092463995564,-8.23871827360899));
#8642=CARTESIAN_POINT('Ctrl Pts',(0.409024941780786,-68.5148232638019,-8.2385633499616));
#8643=CARTESIAN_POINT('Ctrl Pts',(0.543830045690013,-68.5204001280475,-8.23840842631422));
#8644=CARTESIAN_POINT('Ctrl Pts',(0.678393385609739,-68.528732587766,-8.2381805078804));
#8645=CARTESIAN_POINT('Ctrl Pts',(0.812310796291931,-68.5397620635481,-8.23787599113737));
#8646=CARTESIAN_POINT('Ctrl Pts',(0.981838135137693,-68.5537243830754,-8.23749050046207));
#8647=CARTESIAN_POINT('Ctrl Pts',(1.15033458376048,-68.5719977907132,-8.23698101142716));
#8648=CARTESIAN_POINT('Ctrl Pts',(1.31789673537818,-68.5945103285804,-8.23635430529869));
#8649=CARTESIAN_POINT('Ctrl Pts',(1.41506462229892,-68.6075651605497,-8.23599088366895));
#8650=CARTESIAN_POINT('Ctrl Pts',(1.5119184072392,-68.6220464790647,-8.23558813775747));
#8651=CARTESIAN_POINT('Ctrl Pts',(1.60847689897075,-68.6379482314015,-8.23514815153247));
#8652=CARTESIAN_POINT('Ctrl Pts',(1.78446273565371,-68.6669304901292,-8.23434624025003));
#8653=CARTESIAN_POINT('Ctrl Pts',(1.9594583758023,-68.7006270056341,-8.23341922375072));
#8654=CARTESIAN_POINT('Ctrl Pts',(2.1335183778158,-68.7390365074673,-8.23236162604042));
#8655=CARTESIAN_POINT('Ctrl Pts',(2.30698468192499,-68.7773149990713,-8.23130763566975));
#8656=CARTESIAN_POINT('Ctrl Pts',(2.47952223308019,-68.8202745200974,-8.23012397391906));
#8657=CARTESIAN_POINT('Ctrl Pts',(2.65117268232151,-68.8679636632795,-8.22880952393426));
#8658=CARTESIAN_POINT('Ctrl Pts',(2.82221883563617,-68.9154849166886,-8.22749970147462));
#8659=CARTESIAN_POINT('Ctrl Pts',(2.99238462345483,-68.9677027089631,-8.22606003552361));
#8660=CARTESIAN_POINT('Ctrl Pts',(3.16169140425706,-69.0247124774534,-8.22449335732444));
#8661=CARTESIAN_POINT('Ctrl Pts',(3.28911594250015,-69.0676194619865,-8.22331423593804));
#8662=CARTESIAN_POINT('Ctrl Pts',(3.41605288753761,-69.1132483787518,-8.22206469909378));
#8663=CARTESIAN_POINT('Ctrl Pts',(3.54205396079164,-69.1614646919926,-8.22075210685047));
#8664=CARTESIAN_POINT('Ctrl Pts',(3.66805503404568,-69.2096810052334,-8.21943951460716));
#8665=CARTESIAN_POINT('Ctrl Pts',(3.79311985917955,-69.2604845808539,-8.21806383776203));
#8666=CARTESIAN_POINT('Ctrl Pts',(3.91682185879893,-69.3136831042134,-8.21662552408077));
#8667=CARTESIAN_POINT('Ctrl Pts',(4.08469785324958,-69.385878824895,-8.21467358845874));
#8668=CARTESIAN_POINT('Ctrl Pts',(4.25007336704315,-69.4624744124128,-8.21260495076621));
#8669=CARTESIAN_POINT('Ctrl Pts',(4.41300814181022,-69.5434155490575,-8.21042789515496));
#8670=CARTESIAN_POINT('Ctrl Pts',(4.49019533936177,-69.5817598467261,-8.20939655717456));
#8671=CARTESIAN_POINT('Ctrl Pts',(4.5668345824311,-69.621080106923,-8.20834096177747));
#8672=CARTESIAN_POINT('Ctrl Pts',(4.64293089072211,-69.6613743873479,-8.20726237441504));
#8673=CARTESIAN_POINT('Ctrl Pts',(4.8103442668302,-69.750022597429,-8.20488946098699));
#8674=CARTESIAN_POINT('Ctrl Pts',(4.97512450913361,-69.8433787748153,-8.20240389161162));
#8675=CARTESIAN_POINT('Ctrl Pts',(5.13727477281679,-69.9414411800462,-8.19980502327808));
#8676=CARTESIAN_POINT('Ctrl Pts',(5.29870860352638,-70.0390703134527,-8.19721763759604));
#8677=CARTESIAN_POINT('Ctrl Pts',(5.45753612340623,-70.1413645072354,-8.19451799482584));
#8678=CARTESIAN_POINT('Ctrl Pts',(5.6137317611851,-70.2483645458481,-8.19170920857795));
#8679=CARTESIAN_POINT('Ctrl Pts',(5.74433956218909,-70.3378359289754,-8.18936055530861));
#8680=CARTESIAN_POINT('Ctrl Pts',(5.87310679411424,-70.4305984731283,-8.18693566805311));
#8681=CARTESIAN_POINT('Ctrl Pts',(5.99999937459725,-70.5266964145979,-8.18443805265555));
#8682=CARTESIAN_POINT('Ctrl Pts',(5.9999983295249,-70.5266991009391,8.18443799239331));
#8683=CARTESIAN_POINT('Ctrl Pts',(5.86952914135541,-70.4279042693595,8.18700573286285));
#8684=CARTESIAN_POINT('Ctrl Pts',(5.73648042273753,-70.3322021606331,8.1895046414597));
#8685=CARTESIAN_POINT('Ctrl Pts',(5.60141216089113,-70.2399589008432,8.19192377023309));
#8686=CARTESIAN_POINT('Ctrl Pts',(5.53449126469586,-70.1942560722976,8.19312235133062));
#8687=CARTESIAN_POINT('Ctrl Pts',(5.46707376398794,-70.1494025624782,8.19430134521795));
#8688=CARTESIAN_POINT('Ctrl Pts',(5.39922360708421,-70.1054449275604,8.19545938490334));
#8689=CARTESIAN_POINT('Ctrl Pts',(5.25743408344076,-70.0135846813957,8.19787939250308));
#8690=CARTESIAN_POINT('Ctrl Pts',(5.11375652902179,-69.9256335512281,8.20020796766627));
#8691=CARTESIAN_POINT('Ctrl Pts',(4.96827129693732,-69.841514422138,8.20244556438375));
#8692=CARTESIAN_POINT('Ctrl Pts',(4.87803597365184,-69.7893406262195,8.20383340464968));
#8693=CARTESIAN_POINT('Ctrl Pts',(4.78710469185803,-69.7386418773235,8.20518622571968));
#8694=CARTESIAN_POINT('Ctrl Pts',(4.69549237430863,-69.6894088764903,8.20650391776634));
#8695=CARTESIAN_POINT('Ctrl Pts',(4.6762564686983,-69.6790713871409,8.2067805945333));
#8696=CARTESIAN_POINT('Ctrl Pts',(4.65699052868404,-69.6687985443116,8.20705572191943));
#8697=CARTESIAN_POINT('Ctrl Pts',(4.63769388209867,-69.6585901039548,8.20732930453224));
#8698=CARTESIAN_POINT('Ctrl Pts',(4.39017962767364,-69.5276484663706,8.21083849438733));
#8699=CARTESIAN_POINT('Ctrl Pts',(4.13833520205855,-69.4076810004414,8.2140751261655));
#8700=CARTESIAN_POINT('Ctrl Pts',(3.88172272152124,-69.2985071798683,8.21703503037178));
#8701=CARTESIAN_POINT('Ctrl Pts',(3.66073824435755,-69.2044910213058,8.21958398232497));
#8702=CARTESIAN_POINT('Ctrl Pts',(3.43621759575504,-69.1184802024722,8.22192769806047));
#8703=CARTESIAN_POINT('Ctrl Pts',(3.20786877787091,-69.040387840584,8.2240628011651));
#8704=CARTESIAN_POINT('Ctrl Pts',(3.19424339780753,-69.0357281356614,8.22419020095435));
#8705=CARTESIAN_POINT('Ctrl Pts',(3.18060438420692,-69.0310966313511,8.22431685779488));
#8706=CARTESIAN_POINT('Ctrl Pts',(3.16695192959349,-69.0264934493831,8.22444276748959));
#8707=CARTESIAN_POINT('Ctrl Pts',(2.95485023303377,-68.95497937132,8.22639887433025));
#8708=CARTESIAN_POINT('Ctrl Pts',(2.73944418113102,-68.8902852528574,8.22817652038379));
#8709=CARTESIAN_POINT('Ctrl Pts',(2.52171858644569,-68.8329431873267,8.22975681571581));
#8710=CARTESIAN_POINT('Ctrl Pts',(2.48914750906238,-68.8243649911968,8.22999322302301));
#8711=CARTESIAN_POINT('Ctrl Pts',(2.4565245579048,-68.8159512403314,8.23022521610616));
#8712=CARTESIAN_POINT('Ctrl Pts',(2.42385306368375,-68.8077036207449,8.23045273427335));
#8713=CARTESIAN_POINT('Ctrl Pts',(2.41330752868356,-68.8050414969856,8.23052617140418));
#8714=CARTESIAN_POINT('Ctrl Pts',(2.40275693634491,-68.8023966811721,8.23059914232783));
#8715=CARTESIAN_POINT('Ctrl Pts',(2.39220145545524,-68.7997691986063,8.2306716459234));
#8716=CARTESIAN_POINT('Ctrl Pts',(2.15048775697385,-68.739601543971,8.23233193145869));
#8717=CARTESIAN_POINT('Ctrl Pts',(1.90618545878813,-68.6885125030794,8.23374612624222));
#8718=CARTESIAN_POINT('Ctrl Pts',(1.66089102088927,-68.6467302669797,8.23490402309128));
#8719=CARTESIAN_POINT('Ctrl Pts',(1.64754851003194,-68.6444575699566,8.23496700556823));
#8720=CARTESIAN_POINT('Ctrl Pts',(1.63420306192931,-68.6422124215772,8.23502922939213));
#8721=CARTESIAN_POINT('Ctrl Pts',(1.62085493312774,-68.6399948629774,8.23509069279914));
#8722=CARTESIAN_POINT('Ctrl Pts',(1.61374908486424,-68.6388143503259,8.23512341271445));
#8723=CARTESIAN_POINT('Ctrl Pts',(1.60664247690719,-68.637641656468,8.23515591713173));
#8724=CARTESIAN_POINT('Ctrl Pts',(1.59953508414201,-68.6364767804816,8.23518820602338));
#8725=CARTESIAN_POINT('Ctrl Pts',(1.33718455630123,-68.5934784771657,8.23638006470422));
#8726=CARTESIAN_POINT('Ctrl Pts',(1.07384822645327,-68.5611469627105,8.23728059896383));
#8727=CARTESIAN_POINT('Ctrl Pts',(0.808525090100186,-68.539451008081,8.23788453741318));
#8728=CARTESIAN_POINT('Ctrl Pts',(0.804925810356564,-68.5391566884408,8.23789273022839));
#8729=CARTESIAN_POINT('Ctrl Pts',(0.801326165025958,-68.538864325773,8.23790086846902));
#8730=CARTESIAN_POINT('Ctrl Pts',(0.797726162962058,-68.5385739203607,8.23790895211685));
#8731=CARTESIAN_POINT('Ctrl Pts',(0.532630993747636,-68.5171891904231,8.23850421177229));
#8732=CARTESIAN_POINT('Ctrl Pts',(0.265540661321849,-68.5064142752162,8.23880459800998));
#8733=CARTESIAN_POINT('Ctrl Pts',(-3.51073400206478E-10,-68.5063672600388,
8.23880581768755));
#8734=CARTESIAN_POINT('',(6.00000000000001,-8.18443804034558,70.5266968882263));
#8735=CARTESIAN_POINT('Ctrl Pts',(4.16541472538293E-10,-8.23880590935122,
68.5063673993548));
#8736=CARTESIAN_POINT('Ctrl Pts',(0.00416345598546408,-8.23880592987024,
68.506366666553));
#8737=CARTESIAN_POINT('Ctrl Pts',(0.277610744887515,-8.23880245316255,68.5064915939776));
#8738=CARTESIAN_POINT('Ctrl Pts',(0.816727761679238,-8.23816650019571,68.5293033513698));
#8739=CARTESIAN_POINT('Ctrl Pts',(1.61170598678262,-8.23543318022081,68.6275793681561));
#8740=CARTESIAN_POINT('Ctrl Pts',(2.39732558377894,-8.23094391608953,68.7897189261084));
#8741=CARTESIAN_POINT('Ctrl Pts',(3.17804312806208,-8.22465018744083,69.0185952328547));
#8742=CARTESIAN_POINT('Ctrl Pts',(3.92894292458085,-8.21678502129265,69.3072164748245));
#8743=CARTESIAN_POINT('Ctrl Pts',(4.89068866338157,-8.20435137693732,69.768539148429));
#8744=CARTESIAN_POINT('Ctrl Pts',(5.56837676918829,-8.19293364330735,70.1998211121876));
#8745=CARTESIAN_POINT('Ctrl Pts',(6.00000000000001,-8.18443804034558,70.5266968882263));
#8746=CARTESIAN_POINT('',(6.00000079446281,8.18443781970293,70.5266943053403));
#8747=CARTESIAN_POINT('Origin',(6.,0.,0.));
#8748=CARTESIAN_POINT('Ctrl Pts',(6.00000079446281,8.18443781970294,70.5266943053403));
#8749=CARTESIAN_POINT('Ctrl Pts',(5.82155183841513,8.18794923220616,70.3915366584588));
#8750=CARTESIAN_POINT('Ctrl Pts',(5.63916240398924,8.19132108429475,70.2627665326567));
#8751=CARTESIAN_POINT('Ctrl Pts',(5.45240408670687,8.1945511670375,70.1401258483009));
#8752=CARTESIAN_POINT('Ctrl Pts',(5.43621847707622,8.1948311056186,70.1294970620134));
#8753=CARTESIAN_POINT('Ctrl Pts',(5.42000008376334,8.1951099797053,70.118914304163));
#8754=CARTESIAN_POINT('Ctrl Pts',(5.40374864585165,8.19538778805092,70.1083774012658));
#8755=CARTESIAN_POINT('Ctrl Pts',(5.38105594658528,8.19577570580165,70.0936641943519));
#8756=CARTESIAN_POINT('Ctrl Pts',(5.35829881879662,8.19616154554046,70.0790403964617));
#8757=CARTESIAN_POINT('Ctrl Pts',(5.33548081285126,8.19654524000997,70.0645079277786));
#8758=CARTESIAN_POINT('Ctrl Pts',(5.18185112519004,8.19912858851329,69.9666633295222));
#8759=CARTESIAN_POINT('Ctrl Pts',(5.02530020323893,8.20161758690385,69.8728510426696));
#8760=CARTESIAN_POINT('Ctrl Pts',(4.8666174970433,8.20399815192714,69.7835350039511));
#8761=CARTESIAN_POINT('Ctrl Pts',(4.81060345528634,8.20483847707547,69.7520069789867));
#8762=CARTESIAN_POINT('Ctrl Pts',(4.75432336621731,8.20566528575196,69.7210394644626));
#8763=CARTESIAN_POINT('Ctrl Pts',(4.69781078689656,8.20647793764918,69.6906538318512));
#8764=CARTESIAN_POINT('Ctrl Pts',(4.67712257658307,8.20677543448199,69.6795302136139));
#8765=CARTESIAN_POINT('Ctrl Pts',(4.65640320427027,8.20707103395485,69.6684845823009));
#8766=CARTESIAN_POINT('Ctrl Pts',(4.63565284037979,8.20736473752302,69.6575167460913));
#8767=CARTESIAN_POINT('Ctrl Pts',(4.46538751060781,8.20977469694131,69.5675211075104));
#8768=CARTESIAN_POINT('Ctrl Pts',(4.29313372624732,8.21205392334671,69.4828105614274));
#8769=CARTESIAN_POINT('Ctrl Pts',(4.11901696281379,8.21420099130811,69.4033085084354));
#8770=CARTESIAN_POINT('Ctrl Pts',(4.06713153073576,8.21484080074794,69.3796175191864));
#8771=CARTESIAN_POINT('Ctrl Pts',(4.01508053132934,8.21546886660144,69.3563893661196));
#8772=CARTESIAN_POINT('Ctrl Pts',(3.96286696914459,8.21608513032504,69.3336228546209));
#8773=CARTESIAN_POINT('Ctrl Pts',(3.94536666907604,8.21629168202604,69.3259922550972));
#8774=CARTESIAN_POINT('Ctrl Pts',(3.92784810612159,8.21649690782433,69.318413518385));
#8775=CARTESIAN_POINT('Ctrl Pts',(3.91031105586775,8.21670080821778,69.3108865238576));
#8776=CARTESIAN_POINT('Ctrl Pts',(3.67860897710432,8.21939477010644,69.2114387687571));
#8777=CARTESIAN_POINT('Ctrl Pts',(3.44372375805669,8.22185815037421,69.1210462160137));
#8778=CARTESIAN_POINT('Ctrl Pts',(3.20575717391094,8.22408401789359,69.0396653507124));
#8779=CARTESIAN_POINT('Ctrl Pts',(3.19164154379547,8.22421605123223,69.0348380250726));
#8780=CARTESIAN_POINT('Ctrl Pts',(3.17751507598537,8.22434724919125,69.0300423949384));
#8781=CARTESIAN_POINT('Ctrl Pts',(3.16337770078198,8.22447760976305,69.0252784817195));
#8782=CARTESIAN_POINT('Ctrl Pts',(2.9211665930845,8.22671103556112,68.9436598869558));
#8783=CARTESIAN_POINT('Ctrl Pts',(2.67577731324865,8.2286990141984,68.8713564483493));
#8784=CARTESIAN_POINT('Ctrl Pts',(2.42661791252754,8.23043466497516,68.808401884732));
#8785=CARTESIAN_POINT('Ctrl Pts',(2.41606416224099,8.23050818267038,68.8057352916117));
#8786=CARTESIAN_POINT('Ctrl Pts',(2.40550364625273,8.23058124754378,68.8030854757963));
#8787=CARTESIAN_POINT('Ctrl Pts',(2.39493649585478,8.23065385797032,68.8004524833151));
#8788=CARTESIAN_POINT('Ctrl Pts',(2.14155816613234,8.23239490526352,68.7373187895628));
#8789=CARTESIAN_POINT('Ctrl Pts',(1.88427006063706,8.23387456206401,68.6838391773228));
#8790=CARTESIAN_POINT('Ctrl Pts',(1.62517257027932,8.23507095393907,68.6407124984445));
#8791=CARTESIAN_POINT('Ctrl Pts',(1.61835756045793,8.23510242248926,68.6395781426478));
#8792=CARTESIAN_POINT('Ctrl Pts',(1.61154129987145,8.23513369515959,68.6384509459718));
#8793=CARTESIAN_POINT('Ctrl Pts',(1.60472381969236,8.23516477189413,68.6373309098572));
#8794=CARTESIAN_POINT('Ctrl Pts',(1.34152296839364,8.23636454406381,68.5940899394226));
#8795=CARTESIAN_POINT('Ctrl Pts',(1.0765164340326,8.23727044669812,68.561520555236));
#8796=CARTESIAN_POINT('Ctrl Pts',(0.81117025799267,8.23787819074675,68.5396682419934));
#8797=CARTESIAN_POINT('Ctrl Pts',(0.808339331029581,8.2378846746503,68.5394351038955));
#8798=CARTESIAN_POINT('Ctrl Pts',(0.80550836537592,8.23789112460624,68.5392031860196));
#8799=CARTESIAN_POINT('Ctrl Pts',(0.802677360020277,8.23789754061042,68.5389724884737));
#8800=CARTESIAN_POINT('Ctrl Pts',(0.53568415341721,8.23850263643787,68.5172153139734));
#8801=CARTESIAN_POINT('Ctrl Pts',(0.268362014995775,8.23880636303395,68.5063145889559));
#8802=CARTESIAN_POINT('Ctrl Pts',(-2.38940450967676E-10,8.23880549026604,
68.5063639612443));
#8803=CARTESIAN_POINT('Ctrl Pts',(-8.95159733014031E-12,68.5063647597673,
8.23880598322944));
#8804=CARTESIAN_POINT('Ctrl Pts',(0.000821623443402016,68.5063649144486,
8.23880597887183));
#8805=CARTESIAN_POINT('Ctrl Pts',(0.271041635589146,68.5064494487375,8.2388036071868));
#8806=CARTESIAN_POINT('Ctrl Pts',(0.813049986647028,68.5287264288495,8.23818246295993));
#8807=CARTESIAN_POINT('Ctrl Pts',(1.87711179906711,68.6604780686295,8.23451866590537));
#8808=CARTESIAN_POINT('Ctrl Pts',(2.91023424206843,68.9172079362927,8.22741504885044));
#8809=CARTESIAN_POINT('Ctrl Pts',(3.9186730012011,69.3024856616359,8.216912881982));
#8810=CARTESIAN_POINT('Ctrl Pts',(4.89035765134611,69.7679092313649,8.20436742745112));
#8811=CARTESIAN_POINT('Ctrl Pts',(5.56902654677854,70.2003132763431,8.1929208520031));
#8812=CARTESIAN_POINT('Ctrl Pts',(5.99999909300179,70.5266962013408,8.18443805819819));
#8813=CARTESIAN_POINT('Ctrl Pts',(5.99999728414902,70.526700485917,-8.18443796047155));
#8814=CARTESIAN_POINT('Ctrl Pts',(5.88877062295712,70.4424830590272,-8.18662683690695));
#8815=CARTESIAN_POINT('Ctrl Pts',(5.77574490007538,70.3605798226138,-8.18876497800162));
#8816=CARTESIAN_POINT('Ctrl Pts',(5.66125555859731,70.2811701233984,-8.19084582792973));
#8817=CARTESIAN_POINT('Ctrl Pts',(5.57445682198249,70.2209666015868,-8.19242339962779));
#8818=CARTESIAN_POINT('Ctrl Pts',(5.48681542965758,70.1621965864257,-8.19396803945737));
#8819=CARTESIAN_POINT('Ctrl Pts',(5.39846309902672,70.104951809959,-8.19547660000369));
#8820=CARTESIAN_POINT('Ctrl Pts',(5.37712412501396,70.091125974368,-8.19584094958071));
#8821=CARTESIAN_POINT('Ctrl Pts',(5.3557436421719,70.0773891765976,-8.19620319302142));
#8822=CARTESIAN_POINT('Ctrl Pts',(5.33431990260324,70.0637400838969,-8.19656335494725));
#8823=CARTESIAN_POINT('Ctrl Pts',(5.12555734430554,69.9307371830023,-8.20007293481291));
#8824=CARTESIAN_POINT('Ctrl Pts',(4.91298617423999,69.8062578101768,-8.20338216870485));
#8825=CARTESIAN_POINT('Ctrl Pts',(4.6966209436992,69.6900147108326,-8.20649206551354));
#8826=CARTESIAN_POINT('Ctrl Pts',(4.67758612395171,69.6797881765721,-8.20676565995863));
#8827=CARTESIAN_POINT('Ctrl Pts',(4.65852195332554,69.6696253597668,-8.20703771231119));
#8828=CARTESIAN_POINT('Ctrl Pts',(4.63942867597594,69.6595263429874,-8.20730821675026));
#8829=CARTESIAN_POINT('Ctrl Pts',(4.41919463829539,69.5430378428103,-8.21042838746465));
#8830=CARTESIAN_POINT('Ctrl Pts',(4.1948631000602,69.4349201743698,-8.21334228193345));
#8831=CARTESIAN_POINT('Ctrl Pts',(3.9666611220002,69.3352782563471,-8.21603993954926));
#8832=CARTESIAN_POINT('Ctrl Pts',(3.71881052821058,69.2270569834282,-8.21896987051482));
#8833=CARTESIAN_POINT('Ctrl Pts',(3.46639444521359,69.128834043849,-8.22164471824023));
#8834=CARTESIAN_POINT('Ctrl Pts',(3.20863192391708,69.0406490402862,-8.22405548872155));
#8835=CARTESIAN_POINT('Ctrl Pts',(3.1948218931075,69.0359243905969,-8.22418464952606));
#8836=CARTESIAN_POINT('Ctrl Pts',(3.18099651671809,69.0312285512257,-8.22431305238602));
#8837=CARTESIAN_POINT('Ctrl Pts',(3.16715627968411,69.0265616991943,-8.22444069139633));
#8838=CARTESIAN_POINT('Ctrl Pts',(2.92272573864455,68.9441410611525,-8.2266949065714));
#8839=CARTESIAN_POINT('Ctrl Pts',(2.67368605348898,68.8707694212835,-8.22871285737206));
#8840=CARTESIAN_POINT('Ctrl Pts',(2.42264702829873,68.8073992448633,-8.23046107662634));
#8841=CARTESIAN_POINT('Ctrl Pts',(2.41178473411857,68.8046572588394,-8.23053672092832));
#8842=CARTESIAN_POINT('Ctrl Pts',(2.4009186965982,68.8019339994299,-8.23061186018697));
#8843=CARTESIAN_POINT('Ctrl Pts',(2.3900489422933,68.7992294611676,-8.23068649406848));
#8844=CARTESIAN_POINT('Ctrl Pts',(2.13547959455546,68.7358892492317,-8.23243441752685));
#8845=CARTESIAN_POINT('Ctrl Pts',(1.87896849200073,68.6828384134398,-8.23390321081528));
#8846=CARTESIAN_POINT('Ctrl Pts',(1.62076868896401,68.6399805175378,-8.2350913428248));
#8847=CARTESIAN_POINT('Ctrl Pts',(1.61314971826133,68.6387158649338,-8.23512640227436));
#8848=CARTESIAN_POINT('Ctrl Pts',(1.60552927668701,68.6374600903476,-8.23516121726959));
#8849=CARTESIAN_POINT('Ctrl Pts',(1.59790736495981,68.6362131981471,-8.23519578763072));
#8850=CARTESIAN_POINT('Ctrl Pts',(1.33624255857368,68.5934066401744,-8.23638260888731));
#8851=CARTESIAN_POINT('Ctrl Pts',(1.07285116140782,68.5610718339649,-8.23728255736077));
#8852=CARTESIAN_POINT('Ctrl Pts',(0.807971934124623,68.5394056876693,-8.23788571950343));
#8853=CARTESIAN_POINT('Ctrl Pts',(0.803663067258854,68.5390532382121,-8.23789553131615));
#8854=CARTESIAN_POINT('Ctrl Pts',(0.799353806765366,68.5387036113629,-8.23790526460795));
#8855=CARTESIAN_POINT('Ctrl Pts',(0.795044166515618,68.53835680702,-8.23791491937101));
#8856=CARTESIAN_POINT('Ctrl Pts',(0.530457939610201,68.5170650872393,-8.23850766428316));
#8857=CARTESIAN_POINT('Ctrl Pts',(0.264393140237664,68.5064088475944,-8.23880474753574));
#8858=CARTESIAN_POINT('Ctrl Pts',(-2.73511885838946E-10,68.5063670000441,
-8.23880582348961));
#8859=CARTESIAN_POINT('Ctrl Pts',(-3.18401114664506E-12,8.23880597151339,
-68.5063651759543));
#8860=CARTESIAN_POINT('Ctrl Pts',(0.000197208001215656,8.23880597105813,
-68.5063651919466));
#8861=CARTESIAN_POINT('Ctrl Pts',(0.269379031644614,8.23880512607218,-68.5063950399915));
#8862=CARTESIAN_POINT('Ctrl Pts',(0.808562402718581,8.23819328895472,-68.5283381860597));
#8863=CARTESIAN_POINT('Ctrl Pts',(1.87925012401009,8.23451686535867,-68.6605385446451));
#8864=CARTESIAN_POINT('Ctrl Pts',(2.91199036992062,8.22738994814212,-68.9181356819889));
#8865=CARTESIAN_POINT('Ctrl Pts',(3.9138431051418,8.21696851242034,-69.3004357176585));
#8866=CARTESIAN_POINT('Ctrl Pts',(4.89022818173288,8.20437701925203,-69.7675337025404));
#8867=CARTESIAN_POINT('Ctrl Pts',(5.56909800240238,8.19291944450744,-70.2003674353596));
#8868=CARTESIAN_POINT('Ctrl Pts',(5.99999856012047,8.18443806868659,-70.5266957977807));
#8869=CARTESIAN_POINT('Origin',(6.,-81.,6.));
#8870=CARTESIAN_POINT('Origin',(6.,0.,0.));
#8871=CARTESIAN_POINT('Ctrl Pts',(6.,6.00000000000024,68.1397368351434));
#8872=CARTESIAN_POINT('Ctrl Pts',(6.,6.00000000000025,68.4372608978003));
#8873=CARTESIAN_POINT('Ctrl Pts',(6.,6.04965101665905,68.7349461355828));
#8874=CARTESIAN_POINT('Ctrl Pts',(6.,6.2446302212969,69.3064823965443));
#8875=CARTESIAN_POINT('Ctrl Pts',(6.00000000000135,6.39328919939164,69.5806121655312));
#8876=CARTESIAN_POINT('Ctrl Pts',(6.00000000000135,6.76208224766943,70.0282007545523));
#8877=CARTESIAN_POINT('Ctrl Pts',(6.,6.9733548679495,70.2089295378112));
#8878=CARTESIAN_POINT('Ctrl Pts',(6.,7.37004430436642,70.4192718977462));
#8879=CARTESIAN_POINT('Ctrl Pts',(5.99999999998631,7.53536956523719,70.4786001966803));
#8880=CARTESIAN_POINT('Ctrl Pts',(5.99999999998631,7.86537303383998,70.5396271940705));
#8881=CARTESIAN_POINT('Ctrl Pts',(6.,8.02526185723979,70.5451663805613));
#8882=CARTESIAN_POINT('Ctrl Pts',(6.,8.18443767292577,70.5266937224604));
#8883=CARTESIAN_POINT('Ctrl Pts',(6.,-8.1844379396224,70.5267011803182));
#8884=CARTESIAN_POINT('Ctrl Pts',(6.,-8.0258764476141,70.5451008684421));
#8885=CARTESIAN_POINT('Ctrl Pts',(6.00000000003114,-7.86660084437536,70.5396767302592));
#8886=CARTESIAN_POINT('Ctrl Pts',(6.00000000003114,-7.53785118706882,70.4792699334571));
#8887=CARTESIAN_POINT('Ctrl Pts',(6.,-7.37311003018443,70.4204832009684));
#8888=CARTESIAN_POINT('Ctrl Pts',(6.,-6.97693717792651,70.2115400596563));
#8889=CARTESIAN_POINT('Ctrl Pts',(6.00000000000216,-6.76557809943801,70.0315615011381));
#8890=CARTESIAN_POINT('Ctrl Pts',(6.00000000000216,-6.39627772637684,69.5853535340167));
#8891=CARTESIAN_POINT('Ctrl Pts',(6.,-6.24722968116823,69.3118720006602));
#8892=CARTESIAN_POINT('Ctrl Pts',(6.,-6.05037840315953,68.7391559470898));
#8893=CARTESIAN_POINT('Ctrl Pts',(6.,-6.00000402839798,68.4393237078532));
#8894=CARTESIAN_POINT('Ctrl Pts',(6.,-6.00000000024154,68.1396788547224));
#8895=CARTESIAN_POINT('Origin',(-6.,81.,6.));
#8896=CARTESIAN_POINT('Origin',(-6.,1.17789865652746E-16,0.));
#8897=CARTESIAN_POINT('Ctrl Pts',(-6.,68.1397019025295,6.00000000000004));
#8898=CARTESIAN_POINT('Ctrl Pts',(-6.,68.4372486108155,5.99999994767389));
#8899=CARTESIAN_POINT('Ctrl Pts',(-6.,68.734965697874,6.0496595769299));
#8900=CARTESIAN_POINT('Ctrl Pts',(-6.,69.3065130464615,6.24464436565585));
#8901=CARTESIAN_POINT('Ctrl Pts',(-6.00000000000061,69.580625839489,6.39329137641111));
#8902=CARTESIAN_POINT('Ctrl Pts',(-6.00000000000061,70.028203763518,6.76207415119899));
#8903=CARTESIAN_POINT('Ctrl Pts',(-6.00000000027369,70.208928253055,6.97334472427177));
#8904=CARTESIAN_POINT('Ctrl Pts',(-6.00000000027369,70.4192699121286,7.37003273462433));
#8905=CARTESIAN_POINT('Ctrl Pts',(-5.99999999998997,70.4785993003653,7.53536040161822));
#8906=CARTESIAN_POINT('Ctrl Pts',(-5.99999999998997,70.5396278066748,7.86536832103549));
#8907=CARTESIAN_POINT('Ctrl Pts',(-6.,70.5451673858303,8.02525949965797));
#8908=CARTESIAN_POINT('Ctrl Pts',(-6.,70.5266946612721,8.18443778189399));
#8909=CARTESIAN_POINT('Ctrl Pts',(-6.,70.5267027901716,-8.18443790289761));
#8910=CARTESIAN_POINT('Ctrl Pts',(-6.,70.5451026280608,-8.02587206439152));
#8911=CARTESIAN_POINT('Ctrl Pts',(-6.00000000004388,70.5396777866917,-7.86659240106826));
#8912=CARTESIAN_POINT('Ctrl Pts',(-6.00000000004388,70.4792681383387,-7.53783505312272));
#8913=CARTESIAN_POINT('Ctrl Pts',(-6.,70.4204793555461,-7.37308992300955));
#8914=CARTESIAN_POINT('Ctrl Pts',(-6.,70.2115359913312,-6.97692019146415));
#8915=CARTESIAN_POINT('Ctrl Pts',(-6.00000000000371,70.0315643000756,-6.76556755522217));
#8916=CARTESIAN_POINT('Ctrl Pts',(-6.00000000000371,69.5853654206441,-6.3962796681645));
#8917=CARTESIAN_POINT('Ctrl Pts',(-6.,69.3118877775374,-6.24723921228693));
#8918=CARTESIAN_POINT('Ctrl Pts',(-6.,68.739178955923,-6.05038425472732));
#8919=CARTESIAN_POINT('Ctrl Pts',(-6.,68.439335921525,-6.00000474549972));
#8920=CARTESIAN_POINT('Ctrl Pts',(-6.,68.1396788547224,-6.00000000033548));
#8921=CARTESIAN_POINT('Origin',(10.,0.,0.));
#8922=CARTESIAN_POINT('',(-10.,0.,-16.));
#8923=CARTESIAN_POINT('Origin',(-10.,0.,0.));
#8924=CARTESIAN_POINT('',(-8.,-1.95943487863577E-15,-16.));
#8925=CARTESIAN_POINT('',(10.,-1.95943487863577E-15,-16.));
#8926=CARTESIAN_POINT('Origin',(-8.,0.,0.));
#8927=CARTESIAN_POINT('',(8.,-1.95943487863577E-15,-16.));
#8928=CARTESIAN_POINT('Origin',(8.,0.,0.));
#8929=CARTESIAN_POINT('',(10.,0.,-16.));
#8930=CARTESIAN_POINT('',(10.,-1.95943487863577E-15,-16.));
#8931=CARTESIAN_POINT('Origin',(10.,0.,0.));
#8932=CARTESIAN_POINT('Origin',(8.,0.,0.));
#8933=CARTESIAN_POINT('Origin',(-8.,0.,0.));
#8934=CARTESIAN_POINT('Origin',(8.,0.,0.));
#8935=CARTESIAN_POINT('Origin',(-8.,0.,0.));
#8936=CARTESIAN_POINT('Origin',(8.,0.,0.));
#8937=CARTESIAN_POINT('Origin',(-8.,0.,0.));
#8938=CARTESIAN_POINT('Origin',(-7.99999999999999,0.,0.));
#8939=CARTESIAN_POINT('Origin',(8.,0.,0.));
#8940=CARTESIAN_POINT('Origin',(10.,0.,0.));
#8941=CARTESIAN_POINT('',(10.,-6.,6.));
#8942=CARTESIAN_POINT('',(10.,6.,6.));
#8943=CARTESIAN_POINT('',(10.,-6.,6.));
#8944=CARTESIAN_POINT('',(10.,6.,-6.));
#8945=CARTESIAN_POINT('',(10.,6.,6.));
#8946=CARTESIAN_POINT('',(10.,-6.,-6.));
#8947=CARTESIAN_POINT('',(10.,6.,-6.));
#8948=CARTESIAN_POINT('',(10.,-6.,-6.));
#8949=CARTESIAN_POINT('Origin',(-10.,0.,0.));
#8950=CARTESIAN_POINT('',(-10.,6.,6.));
#8951=CARTESIAN_POINT('',(-10.,6.,-6.));
#8952=CARTESIAN_POINT('',(-10.,6.,6.));
#8953=CARTESIAN_POINT('',(-10.,-6.,6.));
#8954=CARTESIAN_POINT('',(-10.,-6.,6.));
#8955=CARTESIAN_POINT('',(-10.,-6.,-6.));
#8956=CARTESIAN_POINT('',(-10.,-6.,-6.));
#8957=CARTESIAN_POINT('',(-10.,6.,-6.));
#8958=CARTESIAN_POINT('Origin',(10.,6.,6.));
#8959=CARTESIAN_POINT('',(10.,6.,6.));
#8960=CARTESIAN_POINT('',(10.,-6.,6.));
#8961=CARTESIAN_POINT('Origin',(10.,-6.,-6.));
#8962=CARTESIAN_POINT('',(10.,-6.,-6.));
#8963=CARTESIAN_POINT('Origin',(10.,6.,-6.));
#8964=CARTESIAN_POINT('',(10.,6.,-6.));
#8965=CARTESIAN_POINT('Origin',(10.,6.,-6.));
#8966=CARTESIAN_POINT('Origin',(8.,0.,0.));
#8967=CARTESIAN_POINT('Origin',(-8.,0.,0.));
#8968=CARTESIAN_POINT('Origin',(-8.,0.,0.));
#8969=CARTESIAN_POINT('Origin',(8.,0.,0.));
#8970=CARTESIAN_POINT('Origin',(8.,0.,0.));
#8971=CARTESIAN_POINT('Origin',(8.,0.,0.));
#8972=CARTESIAN_POINT('Origin',(-8.,0.,0.));
#8973=CARTESIAN_POINT('Origin',(-8.,0.,0.));
#8974=CARTESIAN_POINT('Ctrl Pts',(6.0682882506545,-70.5788750615323,8.18308311042592));
#8975=CARTESIAN_POINT('Ctrl Pts',(5.9459930489019,-70.7379930471477,6.));
#8976=CARTESIAN_POINT('Ctrl Pts',(7.2819459007854,-68.9997880838913,6.));
#8977=CARTESIAN_POINT('Ctrl Pts',(5.85289506900496,-70.4128282844964,8.18739110257159));
#8978=CARTESIAN_POINT('Ctrl Pts',(5.73151885261032,-70.5791653100974,5.99999999999939));
#8979=CARTESIAN_POINT('Ctrl Pts',(7.02347408295405,-68.801131325923,6.));
#8980=CARTESIAN_POINT('Ctrl Pts',(5.40466236457489,-70.0955016700879,8.19569728364092));
#8981=CARTESIAN_POINT('Ctrl Pts',(5.28635953512335,-70.2763620707944,6.00000000000028));
#8982=CARTESIAN_POINT('Ctrl Pts',(6.48559483742278,-68.4215002698136,6.));
#8983=CARTESIAN_POINT('Ctrl Pts',(4.46468935872559,-69.5403906874137,8.21045268554692));
#8984=CARTESIAN_POINT('Ctrl Pts',(4.35736242456404,-69.7487777423901,5.99999999999983));
#8985=CARTESIAN_POINT('Ctrl Pts',(5.35762723050994,-67.7574456427915,6.));
#8986=CARTESIAN_POINT('Ctrl Pts',(3.47443845681706,-69.108155810847,8.22218977274494));
#8987=CARTESIAN_POINT('Ctrl Pts',(3.38589325352388,-69.3410267184102,6.00000000000002));
#8988=CARTESIAN_POINT('Ctrl Pts',(4.16932614817419,-67.2404353101984,6.));
#8989=CARTESIAN_POINT('Ctrl Pts',(2.42716688477256,-68.7967926230682,8.23074835772877));
#8990=CARTESIAN_POINT('Ctrl Pts',(2.36326077208656,-69.0481924834197,6.));
#8991=CARTESIAN_POINT('Ctrl Pts',(2.91260026172825,-66.8680260601435,6.));
#8992=CARTESIAN_POINT('Ctrl Pts',(1.6218304880885,-68.6287353881328,8.23540093540621));
#8993=CARTESIAN_POINT('Ctrl Pts',(1.57815237662727,-68.8903657331695,6.));
#8994=CARTESIAN_POINT('Ctrl Pts',(1.94619658570589,-66.6670266084519,6.));
#8995=CARTESIAN_POINT('Ctrl Pts',(0.810640842823951,-68.5282345115354,8.23819625965817));
#8996=CARTESIAN_POINT('Ctrl Pts',(0.788515249238892,-68.7961066876711,6.));
#8997=CARTESIAN_POINT('Ctrl Pts',(0.972769011388829,-66.5468286047189,6.));
#8998=CARTESIAN_POINT('Ctrl Pts',(-0.0132433122964684,-68.4950325348177,
8.23912191540781));
#8999=CARTESIAN_POINT('Ctrl Pts',(-0.0128812315317467,-68.7649879925767,
6.));
#9000=CARTESIAN_POINT('Ctrl Pts',(-0.0158919747557947,-66.5071198611988,
6.));
#9001=CARTESIAN_POINT('Ctrl Pts',(-0.827108987367283,-68.5298673022841,
8.23815076810972));
#9002=CARTESIAN_POINT('Ctrl Pts',(-0.804540023139105,-68.7976373398413,
6.));
#9003=CARTESIAN_POINT('Ctrl Pts',(-0.992530784840697,-66.5487813885413,
6.));
#9004=CARTESIAN_POINT('Ctrl Pts',(-1.63242644644223,-68.63073424706,8.23534551400686));
#9005=CARTESIAN_POINT('Ctrl Pts',(-1.58848648494722,-68.8922433071613,6.));
#9006=CARTESIAN_POINT('Ctrl Pts',(-1.95891173573081,-66.6694172614361,6.));
#9007=CARTESIAN_POINT('Ctrl Pts',(-2.42769216080527,-68.7970511938874,8.23074135526182));
#9008=CARTESIAN_POINT('Ctrl Pts',(-2.36377796144039,-69.048438722032,6.));
#9009=CARTESIAN_POINT('Ctrl Pts',(-2.91323059296582,-66.8683353480222,6.));
#9010=CARTESIAN_POINT('Ctrl Pts',(-3.21763744666268,-69.0317566304427,8.22428947864325));
#9011=CARTESIAN_POINT('Ctrl Pts',(-3.13559523629935,-69.2692975136533,6.));
#9012=CARTESIAN_POINT('Ctrl Pts',(-3.86116493599712,-67.1490571952379,6.));
#9013=CARTESIAN_POINT('Ctrl Pts',(-3.97822064659548,-69.3282657416192,8.21621403377884));
#9014=CARTESIAN_POINT('Ctrl Pts',(-3.88090592793965,-69.549032366911,6.00000000000002));
#9015=CARTESIAN_POINT('Ctrl Pts',(-4.77386477590747,-67.5037162736474,6.));
#9016=CARTESIAN_POINT('Ctrl Pts',(-4.70828444236236,-69.6838200040427,8.20663923051075));
#9017=CARTESIAN_POINT('Ctrl Pts',(-4.5988151491346,-69.8854869172508,5.99999999999994));
#9018=CARTESIAN_POINT('Ctrl Pts',(-5.64994133086137,-67.9290235661228,6.));
#9019=CARTESIAN_POINT('Ctrl Pts',(-5.40786575147718,-70.0977834228121,8.19563756564667));
#9020=CARTESIAN_POINT('Ctrl Pts',(-5.28954603953759,-70.2785444703306,6.00000000000021));
#9021=CARTESIAN_POINT('Ctrl Pts',(-6.48943890167358,-68.4242300266046,6.));
#9022=CARTESIAN_POINT('Ctrl Pts',(-5.85541803997558,-70.4145999513425,8.18734468717341));
#9023=CARTESIAN_POINT('Ctrl Pts',(-5.73401743225063,-70.5808509979729,5.99999999999954));
#9024=CARTESIAN_POINT('Ctrl Pts',(-7.02650164818409,-68.8032508361093,6.));
#9025=CARTESIAN_POINT('Ctrl Pts',(-6.07230111177522,-70.5819701972286,8.18300281304048));
#9026=CARTESIAN_POINT('Ctrl Pts',(-5.94998411612338,-70.7409501459778,6.));
#9027=CARTESIAN_POINT('Ctrl Pts',(-7.28676133413026,-69.0034910751822,6.));
#9028=CARTESIAN_POINT('Ctrl Pts',(-6.06803252706027,-70.5786779305751,-8.18308822489702));
#9029=CARTESIAN_POINT('Ctrl Pts',(-5.94573871849779,-70.7378047103369,-6.));
#9030=CARTESIAN_POINT('Ctrl Pts',(-7.28163903247233,-68.9995522383246,-6.));
#9031=CARTESIAN_POINT('Ctrl Pts',(-5.85347731350505,-70.4132881638106,-8.1873791998786));
#9032=CARTESIAN_POINT('Ctrl Pts',(-5.73210035380063,-70.579606412197,-5.99999999999983));
#9033=CARTESIAN_POINT('Ctrl Pts',(-7.02417277625494,-68.8016815272326,-6.));
#9034=CARTESIAN_POINT('Ctrl Pts',(-5.4111283081438,-70.0998002542412,-8.19558414953762));
#9035=CARTESIAN_POINT('Ctrl Pts',(-5.29276551111711,-70.2804580835622,-6.00000000000008));
#9036=CARTESIAN_POINT('Ctrl Pts',(-6.49335396974988,-68.4266427135835,-6.));
#9037=CARTESIAN_POINT('Ctrl Pts',(-4.70118346556066,-69.6796411462325,-8.20675036532539));
#9038=CARTESIAN_POINT('Ctrl Pts',(-4.59178484404709,-69.8815086667827,-5.99999999999998));
#9039=CARTESIAN_POINT('Ctrl Pts',(-5.64142015867887,-67.9240245960956,-6.));
#9040=CARTESIAN_POINT('Ctrl Pts',(-3.96654205942963,-69.3231600030763,-8.21635249184322));
#9041=CARTESIAN_POINT('Ctrl Pts',(-3.86944503708174,-69.5442114415875,-6.));
#9042=CARTESIAN_POINT('Ctrl Pts',(-4.75985047131393,-67.4976090926177,-6.));
#9043=CARTESIAN_POINT('Ctrl Pts',(-3.20951506433543,-69.0293095986277,-8.22435673696605));
#9044=CARTESIAN_POINT('Ctrl Pts',(-3.12767187365864,-69.2669987740208,-6.));
#9045=CARTESIAN_POINT('Ctrl Pts',(-3.85141807720296,-67.1461303958146,-6.));
#9046=CARTESIAN_POINT('Ctrl Pts',(-2.43078328288814,-68.7978816199521,-8.23071847511551));
#9047=CARTESIAN_POINT('Ctrl Pts',(-2.36679776159459,-69.0492202784216,-6.));
#9048=CARTESIAN_POINT('Ctrl Pts',(-2.91693993946566,-66.8693285762601,-6.));
#9049=CARTESIAN_POINT('Ctrl Pts',(-1.62586716451067,-68.6292738987564,-8.23538592349982));
#9050=CARTESIAN_POINT('Ctrl Pts',(-1.58208021199484,-68.8908695978791,-6.));
#9051=CARTESIAN_POINT('Ctrl Pts',(-1.95104059741283,-66.6676706545943,-6.));
#9052=CARTESIAN_POINT('Ctrl Pts',(-0.811246104747758,-68.528376006915,-8.23819232856168));
#9053=CARTESIAN_POINT('Ctrl Pts',(-0.789104003287774,-68.7962395994468,
-6.));
#9054=CARTESIAN_POINT('Ctrl Pts',(-0.973495325697306,-66.5469978325812,
-6.));
#9055=CARTESIAN_POINT('Ctrl Pts',(0.00694046074342192,-68.4949754898681,
-8.23912350096698));
#9056=CARTESIAN_POINT('Ctrl Pts',(0.0067491433536535,-68.7649343963049,
-6.));
#9057=CARTESIAN_POINT('Ctrl Pts',(0.00832855289212235,-66.5070516358273,
-6.));
#9058=CARTESIAN_POINT('Ctrl Pts',(0.830469565512463,-68.5299319685166,-8.23814897045333));
#9059=CARTESIAN_POINT('Ctrl Pts',(0.80780778884349,-68.7976980585048,-6.));
#9060=CARTESIAN_POINT('Ctrl Pts',(0.996563478614889,-66.5488587288769,-6.));
#9061=CARTESIAN_POINT('Ctrl Pts',(1.63747646581493,-68.6315544877087,-8.23532268183347));
#9062=CARTESIAN_POINT('Ctrl Pts',(1.59340092659167,-68.8930115216497,-6.));
#9063=CARTESIAN_POINT('Ctrl Pts',(1.96497175897817,-66.6703982568214,-6.));
#9064=CARTESIAN_POINT('Ctrl Pts',(2.43210940714635,-68.7983855401701,-8.23070470254197));
#9065=CARTESIAN_POINT('Ctrl Pts',(2.36810398473332,-69.0496973102161,-6.));
#9066=CARTESIAN_POINT('Ctrl Pts',(2.91853128857469,-66.8699313126498,-6.));
#9067=CARTESIAN_POINT('Ctrl Pts',(3.21272958292764,-69.0301041506723,-8.22433471552509));
#9068=CARTESIAN_POINT('Ctrl Pts',(3.13079385880829,-69.2677406291319,-6.00000000000001));
#9069=CARTESIAN_POINT('Ctrl Pts',(3.85527549951665,-67.1470806885609,-6.));
#9070=CARTESIAN_POINT('Ctrl Pts',(3.98172154951034,-69.3295276483392,-8.21617950273701));
#9071=CARTESIAN_POINT('Ctrl Pts',(3.88432273738468,-69.5502163162855,-5.99999999999995));
#9072=CARTESIAN_POINT('Ctrl Pts',(4.77806585939939,-67.5052256260813,-6.));
#9073=CARTESIAN_POINT('Ctrl Pts',(4.95801912054651,-69.8059991662796,-8.20334997367537));
#9074=CARTESIAN_POINT('Ctrl Pts',(4.84354578298823,-70.0007101356207,-6.00000000000025));
#9075=CARTESIAN_POINT('Ctrl Pts',(5.94962294472498,-68.0751721643964,-6.));
#9076=CARTESIAN_POINT('Ctrl Pts',(5.64014398919804,-70.2485011895088,-8.19165365412494));
#9077=CARTESIAN_POINT('Ctrl Pts',(5.51914430293978,-70.4215908515748,-5.99999999999891));
#9078=CARTESIAN_POINT('Ctrl Pts',(6.76817278673088,-68.6045318062231,-6.));
#9079=CARTESIAN_POINT('Ctrl Pts',(6.07195815035803,-70.5817055432315,-8.18300967865433));
#9080=CARTESIAN_POINT('Ctrl Pts',(5.94964301231408,-70.740697292135,-6.));
#9081=CARTESIAN_POINT('Ctrl Pts',(7.28634978042964,-69.0031744455552,-6.));
#9082=CARTESIAN_POINT('Ctrl Pts',(6.06801845291636,8.1830885063712,70.578667081549));
#9083=CARTESIAN_POINT('Ctrl Pts',(5.94572472104539,6.00000000000025,70.7377943453019));
#9084=CARTESIAN_POINT('Ctrl Pts',(7.28162214349963,6.00000000000024,68.9995392586552));
#9085=CARTESIAN_POINT('Ctrl Pts',(5.85350545654079,8.18737862287716,70.4133104642334));
#9086=CARTESIAN_POINT('Ctrl Pts',(5.73212846769281,5.99999999999972,70.579627806427));
#9087=CARTESIAN_POINT('Ctrl Pts',(7.02420654789107,6.00000000000024,68.8017082075856));
#9088=CARTESIAN_POINT('Ctrl Pts',(5.41142083747605,8.19557825641887,70.1000263112598));
#9089=CARTESIAN_POINT('Ctrl Pts',(5.29305834816035,6.0000000000005,70.280674868654));
#9090=CARTESIAN_POINT('Ctrl Pts',(6.49370500495172,6.00000000000024,68.4269131601669));
#9091=CARTESIAN_POINT('Ctrl Pts',(4.70226077585541,8.2067352102742,69.680206595972));
#9092=CARTESIAN_POINT('Ctrl Pts',(4.59284510950782,6.00000000000018,69.8820441142854));
#9093=CARTESIAN_POINT('Ctrl Pts',(5.64271293103173,6.00000000000024,67.9247009918506));
#9094=CARTESIAN_POINT('Ctrl Pts',(3.96640109231569,8.21635488943785,69.3230697140021));
#9095=CARTESIAN_POINT('Ctrl Pts',(3.86930402127679,6.00000000000027,69.5441249357653));
#9096=CARTESIAN_POINT('Ctrl Pts',(4.75968131077742,6.00000000000024,67.497501083266));
#9097=CARTESIAN_POINT('Ctrl Pts',(3.20933677074826,8.22435834530184,69.0292514433744));
#9098=CARTESIAN_POINT('Ctrl Pts',(3.12749804869432,6.00000000000024,69.2669443838855));
#9099=CARTESIAN_POINT('Ctrl Pts',(3.85120412489829,6.00000000000023,67.1460608406989));
#9100=CARTESIAN_POINT('Ctrl Pts',(2.43079492950821,8.23071752336813,68.7979164367695));
#9101=CARTESIAN_POINT('Ctrl Pts',(2.36681062468134,6.00000000000025,69.0492532338038));
#9102=CARTESIAN_POINT('Ctrl Pts',(2.91695391540976,6.00000000000023,66.8693702204437));
#9103=CARTESIAN_POINT('Ctrl Pts',(1.62719099386776,8.23537981519032,68.6294940882333));
#9104=CARTESIAN_POINT('Ctrl Pts',(1.5833700332159,6.00000000000025,68.8910763437912));
#9105=CARTESIAN_POINT('Ctrl Pts',(1.95262919264134,6.00000000000024,66.6679340024137));
#9106=CARTESIAN_POINT('Ctrl Pts',(0.811476579102376,8.23819216142386,68.5283818247723));
#9107=CARTESIAN_POINT('Ctrl Pts',(0.789327567123226,6.00000000000025,68.7962449283322));
#9108=CARTESIAN_POINT('Ctrl Pts',(0.973771894922848,6.00000000000023,66.5470047895178));
#9109=CARTESIAN_POINT('Ctrl Pts',(-0.00607573808073577,8.23912316054545,
68.494987768917));
#9110=CARTESIAN_POINT('Ctrl Pts',(-0.00590784164394143,6.00000000000025,
68.764945955377));
#9111=CARTESIAN_POINT('Ctrl Pts',(-0.007290885696897,6.00000000000023,66.5070663216835));
#9112=CARTESIAN_POINT('Ctrl Pts',(-0.830079220669207,8.23815058533074,68.5298739460195));
#9113=CARTESIAN_POINT('Ctrl Pts',(-0.807427697439417,6.00000000000025,68.7976436237591));
#9114=CARTESIAN_POINT('Ctrl Pts',(-0.996095064802989,6.00000000000023,66.5487893348009));
#9115=CARTESIAN_POINT('Ctrl Pts',(-1.63783143137718,8.23532139951924,68.6316004941713));
#9116=CARTESIAN_POINT('Ctrl Pts',(-1.59374595912617,6.00000000000025,68.8930545679141));
#9117=CARTESIAN_POINT('Ctrl Pts',(-1.96539771765284,6.00000000000024,66.670453279486));
#9118=CARTESIAN_POINT('Ctrl Pts',(-2.4324940845882,8.23070164698601,68.7984964593138));
#9119=CARTESIAN_POINT('Ctrl Pts',(-2.36848014491559,6.00000000000025,69.0498017139277));
#9120=CARTESIAN_POINT('Ctrl Pts',(-2.91899290150501,6.00000000000023,66.8700639772304));
#9121=CARTESIAN_POINT('Ctrl Pts',(-3.21237058587918,8.22433751057345,69.0300029226234));
#9122=CARTESIAN_POINT('Ctrl Pts',(-3.13044430354236,6.00000000000025,69.2676458481511));
#9123=CARTESIAN_POINT('Ctrl Pts',(-3.85484470305812,6.00000000000024,67.1469596163795));
#9124=CARTESIAN_POINT('Ctrl Pts',(-3.98123403834483,8.21618579285133,69.3292945527418));
#9125=CARTESIAN_POINT('Ctrl Pts',(-3.88384257406888,6.00000000000025,69.5499954728079));
#9126=CARTESIAN_POINT('Ctrl Pts',(-4.77748084600222,6.00000000000024,67.5049468043074));
#9127=CARTESIAN_POINT('Ctrl Pts',(-4.9587261495966,8.20334062563248,69.8063458318945));
#9128=CARTESIAN_POINT('Ctrl Pts',(-4.84423794709568,6.00000000000025,70.001036400311));
#9129=CARTESIAN_POINT('Ctrl Pts',(-5.95047137957739,6.00000000000024,68.0755868366564));
#9130=CARTESIAN_POINT('Ctrl Pts',(-5.64048203786072,8.19164677753803,70.2487667358696));
#9131=CARTESIAN_POINT('Ctrl Pts',(-5.51948258067411,6.00000000000029,70.4218460646259));
#9132=CARTESIAN_POINT('Ctrl Pts',(-6.76857844516023,6.00000000000024,68.6048495059982));
#9133=CARTESIAN_POINT('Ctrl Pts',(-6.07190402898392,8.1830107620393,70.5816637813997));
#9134=CARTESIAN_POINT('Ctrl Pts',(-5.94958918416741,6.00000000000025,70.7406573923915));
#9135=CARTESIAN_POINT('Ctrl Pts',(-7.2862848347807,6.00000000000024,69.0031244820821));
#9136=CARTESIAN_POINT('Ctrl Pts',(-6.06834088416797,-8.18308205771751,70.5789156370285));
#9137=CARTESIAN_POINT('Ctrl Pts',(-5.94604539573102,-5.99999999999975,70.7380318125804));
#9138=CARTESIAN_POINT('Ctrl Pts',(-7.28200906100156,-5.99999999999976,68.9998366280225));
#9139=CARTESIAN_POINT('Ctrl Pts',(-5.85277105864604,-8.18739363605577,70.4127304061065));
#9140=CARTESIAN_POINT('Ctrl Pts',(-5.73139500673848,-6.00000000000109,70.5790714320876));
#9141=CARTESIAN_POINT('Ctrl Pts',(-7.02332527052808,-5.99999999999976,68.8010142238958));
#9142=CARTESIAN_POINT('Ctrl Pts',(-5.40389248678053,-8.1957102200564,70.0950123273115));
#9143=CARTESIAN_POINT('Ctrl Pts',(-5.28559866593569,-5.99999999999914,70.2758971643673));
#9144=CARTESIAN_POINT('Ctrl Pts',(-6.48467098406741,-5.99999999999976,68.4209148757263));
#9145=CARTESIAN_POINT('Ctrl Pts',(-4.46552260677635,-8.21043868494446,69.5409186810962));
#9146=CARTESIAN_POINT('Ctrl Pts',(-4.35819209250992,-6.00000000000011,69.7492824480618));
#9147=CARTESIAN_POINT('Ctrl Pts',(-5.3586271281721,-5.99999999999976,67.7580772654495));
#9148=CARTESIAN_POINT('Ctrl Pts',(-3.4753489624829,-8.22218339603287,69.1083854232455));
#9149=CARTESIAN_POINT('Ctrl Pts',(-3.38677700455703,-5.9999999999997,69.3412405452436));
#9150=CARTESIAN_POINT('Ctrl Pts',(-4.170418754973,-5.99999999999977,67.2407099265433));
#9151=CARTESIAN_POINT('Ctrl Pts',(-2.42624705360006,-8.23075476367214,68.7965605885707));
#9152=CARTESIAN_POINT('Ctrl Pts',(-2.36236305382706,-5.99999999999976,69.0479744163574));
#9153=CARTESIAN_POINT('Ctrl Pts',(-2.91149646432129,-5.99999999999977,66.8677485388432));
#9154=CARTESIAN_POINT('Ctrl Pts',(-1.62204779908062,-8.23539943445322,68.6287897669284));
#9155=CARTESIAN_POINT('Ctrl Pts',(-1.57836506118308,-5.99999999999975,68.8904169809383));
#9156=CARTESIAN_POINT('Ctrl Pts',(-1.94645735889641,-5.99999999999977,66.6670916474468));
#9157=CARTESIAN_POINT('Ctrl Pts',(-0.810375770559074,-8.23819731057242,
68.5281966361225));
#9158=CARTESIAN_POINT('Ctrl Pts',(-0.78825681439635,-5.99999999999975,68.796071073066));
#9159=CARTESIAN_POINT('Ctrl Pts',(-0.972450924670978,-5.99999999999977,
66.5467833055616));
#9160=CARTESIAN_POINT('Ctrl Pts',(0.0133055089948572,-8.23912127759622,
68.4950554619354));
#9161=CARTESIAN_POINT('Ctrl Pts',(0.0129415792074661,-5.99999999999975,
68.7650095211385));
#9162=CARTESIAN_POINT('Ctrl Pts',(0.0159666107938615,-5.99999999999977,
66.5071472817672));
#9163=CARTESIAN_POINT('Ctrl Pts',(0.826267631217788,-8.23815227908787,68.529813087084));
#9164=CARTESIAN_POINT('Ctrl Pts',(0.803721811298467,-5.99999999999975,68.7975865283896));
#9165=CARTESIAN_POINT('Ctrl Pts',(0.991521157461304,-5.99999999999977,66.5487165483907));
#9166=CARTESIAN_POINT('Ctrl Pts',(1.63154625951178,-8.23534985135178,68.6305780621835));
#9167=CARTESIAN_POINT('Ctrl Pts',(1.58762892121974,-5.99999999999975,68.8920967742542));
#9168=CARTESIAN_POINT('Ctrl Pts',(1.95785551141427,-5.99999999999977,66.6692304644635));
#9169=CARTESIAN_POINT('Ctrl Pts',(2.42740394362686,-8.23074402945943,68.7969536012691));
#9170=CARTESIAN_POINT('Ctrl Pts',(2.36349505098862,-5.99999999999975,69.0483465087462));
#9171=CARTESIAN_POINT('Ctrl Pts',(2.91288473235175,-5.99999999999976,66.8682186195194));
#9172=CARTESIAN_POINT('Ctrl Pts',(3.21782649539177,-8.22428729467809,69.0318370973241));
#9173=CARTESIAN_POINT('Ctrl Pts',(3.13578143863181,-5.99999999999976,69.2693737863226));
#9174=CARTESIAN_POINT('Ctrl Pts',(3.86139179447194,-5.99999999999977,67.1491534445295));
#9175=CARTESIAN_POINT('Ctrl Pts',(3.97730474384737,-8.21622429420431,69.3278879313072));
#9176=CARTESIAN_POINT('Ctrl Pts',(3.880008753726,-5.99999999999972,69.5486760172004));
#9177=CARTESIAN_POINT('Ctrl Pts',(4.77276569261006,-5.99999999999977,67.5032643626668));
#9178=CARTESIAN_POINT('Ctrl Pts',(4.70742733158002,-8.20665165144787,69.6833563763738));
#9179=CARTESIAN_POINT('Ctrl Pts',(4.59797063943759,-5.99999999999986,69.8850477806615));
#9180=CARTESIAN_POINT('Ctrl Pts',(5.64891279792138,-5.99999999999976,67.9284689696251));
#9181=CARTESIAN_POINT('Ctrl Pts',(5.40725025962937,-8.19564900701384,70.0973460631149));
#9182=CARTESIAN_POINT('Ctrl Pts',(5.28893319868001,-5.99999999999934,70.2781260183458));
#9183=CARTESIAN_POINT('Ctrl Pts',(6.48870031146062,-5.99999999999976,68.4237067935522));
#9184=CARTESIAN_POINT('Ctrl Pts',(5.85561464211331,-8.18734066811789,70.4147552346278));
#9185=CARTESIAN_POINT('Ctrl Pts',(5.73421377853935,-6.00000000000062,70.5809999378274));
#9186=CARTESIAN_POINT('Ctrl Pts',(7.02673757073987,-5.99999999999976,68.8034366175773));
#9187=CARTESIAN_POINT('Ctrl Pts',(6.07221930260315,-8.183004450797,70.5819070651678));
#9188=CARTESIAN_POINT('Ctrl Pts',(5.94990274997528,-5.99999999999975,70.7408898287435));
#9189=CARTESIAN_POINT('Ctrl Pts',(7.28666316312378,-5.99999999999976,69.0034155445595));
#9190=CARTESIAN_POINT('Ctrl Pts',(6.06875473483189,-8.18309759645187,-70.5792319349097));
#9191=CARTESIAN_POINT('Ctrl Pts',(5.94643964085432,-6.00000000000025,-70.7383565071141));
#9192=CARTESIAN_POINT('Ctrl Pts',(7.28250408242006,-6.00000000000024,-69.0002171181955));
#9193=CARTESIAN_POINT('Ctrl Pts',(5.85178703948071,-8.18743757171489,-70.4119510234682));
#9194=CARTESIAN_POINT('Ctrl Pts',(5.73039546650288,-5.99999999999948,-70.5783470003785));
#9195=CARTESIAN_POINT('Ctrl Pts',(7.02214286219319,-6.00000000000024,-68.8000839347804));
#9196=CARTESIAN_POINT('Ctrl Pts',(5.40413875921895,-8.19572501730264,-70.095371489302));
#9197=CARTESIAN_POINT('Ctrl Pts',(5.28584267076014,-6.00000000000061,-70.2762746863069));
#9198=CARTESIAN_POINT('Ctrl Pts',(6.48496496950678,-6.00000000000024,-68.4213469913216));
#9199=CARTESIAN_POINT('Ctrl Pts',(4.70453541541043,-8.20671705513184,-69.6818030748008));
#9200=CARTESIAN_POINT('Ctrl Pts',(4.59510783781567,-6.00000000000016,-69.8836011976203));
#9201=CARTESIAN_POINT('Ctrl Pts',(5.64544107697617,-6.00000000000024,-67.9266134977138));
#9202=CARTESIAN_POINT('Ctrl Pts',(3.97447865414692,-8.21628193502219,-69.3266412584454));
#9203=CARTESIAN_POINT('Ctrl Pts',(3.87722246833469,-6.00000000000028,-69.5475251536455));
#9204=CARTESIAN_POINT('Ctrl Pts',(4.76937312491094,-6.00000000000024,-67.5017760124435));
#9205=CARTESIAN_POINT('Ctrl Pts',(3.21437312354095,-8.22434380390216,-69.0306454426741));
#9206=CARTESIAN_POINT('Ctrl Pts',(3.13239258384128,-6.00000000000024,-69.2682791211047));
#9207=CARTESIAN_POINT('Ctrl Pts',(3.85724668850695,-6.00000000000024,-67.1477311850147));
#9208=CARTESIAN_POINT('Ctrl Pts',(2.42376825729524,-8.23079411637547,-68.7960041651443));
#9209=CARTESIAN_POINT('Ctrl Pts',(2.35993781294462,-6.00000000000025,-69.0474823212491));
#9210=CARTESIAN_POINT('Ctrl Pts',(2.9085210851309,-6.00000000000024,-66.8670862868854));
#9211=CARTESIAN_POINT('Ctrl Pts',(1.62381972536018,-8.2354160205023,-68.6290551598252));
#9212=CARTESIAN_POINT('Ctrl Pts',(1.58008663699865,-6.00000000000025,-68.8906963954579));
#9213=CARTESIAN_POINT('Ctrl Pts',(1.94858310686874,-6.00000000000023,-66.6674124238467));
#9214=CARTESIAN_POINT('Ctrl Pts',(0.806804782644178,-8.238230881506,-68.527846491126));
#9215=CARTESIAN_POINT('Ctrl Pts',(0.784779198305824,-6.00000000000025,-68.795769877695));
#9216=CARTESIAN_POINT('Ctrl Pts',(0.96816545556796,-6.00000000000023,-66.5463679508953));
#9217=CARTESIAN_POINT('Ctrl Pts',(-0.283444643618167,-8.23943970404702,
-68.4845142474358));
#9218=CARTESIAN_POINT('Ctrl Pts',(-0.275801169709708,-6.00000000000025,
-68.7551714931309));
#9219=CARTESIAN_POINT('Ctrl Pts',(-0.340133473956596,-6.00000000000023,
-66.4945438531381));
#9220=CARTESIAN_POINT('Ctrl Pts',(-1.62860970393417,-8.23633611996313,-68.595645744352));
#9221=CARTESIAN_POINT('Ctrl Pts',(-1.58330020161186,-6.00000000000027,-68.8591514885485));
#9222=CARTESIAN_POINT('Ctrl Pts',(-1.9543310609976,-6.00000000000023,-66.6274531349024));
#9223=CARTESIAN_POINT('Ctrl Pts',(-3.2312143093488,-8.22512639339453,-69.0008899721718));
#9224=CARTESIAN_POINT('Ctrl Pts',(-3.14620792364501,-6.00000000000017,-69.2394478237357));
#9225=CARTESIAN_POINT('Ctrl Pts',(-3.87745607258566,-6.00000000000024,-67.1121341857481));
#9226=CARTESIAN_POINT('Ctrl Pts',(-4.46858440416536,-8.21042143575268,-69.5424343805895));
#9227=CARTESIAN_POINT('Ctrl Pts',(-4.36118635957745,-6.00000000000049,-69.7507353701984));
#9228=CARTESIAN_POINT('Ctrl Pts',(-5.36229989129301,-6.00000000000024,-67.759892952126));
#9229=CARTESIAN_POINT('Ctrl Pts',(-5.4083833220806,-8.19565805801412,-70.0978905482687));
#9230=CARTESIAN_POINT('Ctrl Pts',(-5.29002494401106,-5.99999999999985,-70.2786591175671));
#9231=CARTESIAN_POINT('Ctrl Pts',(-6.49005844414082,-6.00000000000024,-68.4243604294078));
#9232=CARTESIAN_POINT('Ctrl Pts',(-5.85649506183581,-8.18734650418252,-70.4154478176525));
#9233=CARTESIAN_POINT('Ctrl Pts',(-5.73507620737369,-6.00000000000114,-70.5816873084557));
#9234=CARTESIAN_POINT('Ctrl Pts',(-7.0277924885399,-6.00000000000024,-68.8042673910917));
#9235=CARTESIAN_POINT('Ctrl Pts',(-6.07185145156228,-8.18303563075614,-70.5816204501341));
#9236=CARTESIAN_POINT('Ctrl Pts',(-5.94951953188762,-6.00000000000025,-70.7406384910899));
#9237=CARTESIAN_POINT('Ctrl Pts',(-7.28622014224927,-6.00000000000024,-69.0030747140361));
#9238=CARTESIAN_POINT('Ctrl Pts',(-6.06801871741568,8.18308850108089,-70.5786672854375));
#9239=CARTESIAN_POINT('Ctrl Pts',(-5.94572498410341,5.99999999999975,-70.7377945400946));
#9240=CARTESIAN_POINT('Ctrl Pts',(-7.28162246089882,5.99999999999976,-68.9995395025853));
#9241=CARTESIAN_POINT('Ctrl Pts',(-5.6389103743372,8.19167038155535,-70.2478905485423));
#9242=CARTESIAN_POINT('Ctrl Pts',(-5.51794464646817,6.00000000000053,-70.4210261561648));
#9243=CARTESIAN_POINT('Ctrl Pts',(-6.76669244916325,5.99999999999976,-68.6038014271042));
#9244=CARTESIAN_POINT('Ctrl Pts',(-4.95704234660675,8.20338648207493,-69.8045805431969));
#9245=CARTESIAN_POINT('Ctrl Pts',(-4.84250783046514,5.99999999999957,-69.9993321538736));
#9246=CARTESIAN_POINT('Ctrl Pts',(-5.94845081593742,5.99999999999976,-68.0734748718918));
#9247=CARTESIAN_POINT('Ctrl Pts',(-3.96744158691016,8.21634812748047,-69.3233047664328));
#9248=CARTESIAN_POINT('Ctrl Pts',(-3.87030741903311,5.99999999999978,-69.5443375003731));
#9249=CARTESIAN_POINT('Ctrl Pts',(-4.76092990429044,5.99999999999976,-67.4977821572228));
#9250=CARTESIAN_POINT('Ctrl Pts',(-3.20874982183398,8.22436433780971,-69.0290350135615));
#9251=CARTESIAN_POINT('Ctrl Pts',(-3.12692407346289,5.99999999999974,-69.2667420899));
#9252=CARTESIAN_POINT('Ctrl Pts',(-3.85049978620124,5.99999999999977,-67.1458019863229));
#9253=CARTESIAN_POINT('Ctrl Pts',(-2.43024294402271,8.23071770241596,-68.7979113655376));
#9254=CARTESIAN_POINT('Ctrl Pts',(-2.36627888415488,5.99999999999975,-69.0492494521875));
#9255=CARTESIAN_POINT('Ctrl Pts',(-2.91629153282712,5.99999999999976,-66.8693641637389));
#9256=CARTESIAN_POINT('Ctrl Pts',(-1.63363652776448,8.23534766361698,-68.6306536433433));
#9257=CARTESIAN_POINT('Ctrl Pts',(-1.5896523597654,5.99999999999975,-68.8921654789989));
#9258=CARTESIAN_POINT('Ctrl Pts',(-1.96036383331742,5.99999999999977,-66.669320840075));
#9259=CARTESIAN_POINT('Ctrl Pts',(-0.815211414748784,8.23818669105861,-68.5285770148599));
#9260=CARTESIAN_POINT('Ctrl Pts',(-0.792958661983601,5.99999999999975,-68.7964271193057));
#9261=CARTESIAN_POINT('Ctrl Pts',(-0.978253697698524,5.99999999999977,-66.5472382258622));
#9262=CARTESIAN_POINT('Ctrl Pts',(0.00264516296727683,8.23912024758092,
-68.495093664448));
#9263=CARTESIAN_POINT('Ctrl Pts',(0.00257169497954889,5.99999999999975,
-68.7650461932855));
#9264=CARTESIAN_POINT('Ctrl Pts',(0.00317419556070009,5.99999999999977,
-66.5071929785566));
#9265=CARTESIAN_POINT('Ctrl Pts',(0.82368949116962,8.23816805427952,-68.5292427295882));
#9266=CARTESIAN_POINT('Ctrl Pts',(0.801208987662387,5.99999999999975,-68.797049035209));
#9267=CARTESIAN_POINT('Ctrl Pts',(0.988427389403655,5.99999999999977,-66.5480343879385));
#9268=CARTESIAN_POINT('Ctrl Pts',(1.91030037741018,8.23437068737471,-68.6658024039292));
#9269=CARTESIAN_POINT('Ctrl Pts',(1.85869062009036,5.99999999999975,-68.9251108313631));
#9270=CARTESIAN_POINT('Ctrl Pts',(2.29236045289163,5.99999999999977,-66.7113585312388));
#9271=CARTESIAN_POINT('Ctrl Pts',(2.9578869124087,8.22702280389032,-68.9314459585039));
#9272=CARTESIAN_POINT('Ctrl Pts',(2.88034732575977,5.99999999999977,-69.1744069005992));
#9273=CARTESIAN_POINT('Ctrl Pts',(3.54946429489408,5.99999999999977,-67.0290743581477));
#9274=CARTESIAN_POINT('Ctrl Pts',(3.9746715687375,8.21626478748155,-69.3263736287728));
#9275=CARTESIAN_POINT('Ctrl Pts',(3.87739899030771,5.99999999999972,-69.5472323185878));
#9276=CARTESIAN_POINT('Ctrl Pts',(4.76960588247878,5.99999999999976,-67.5014529227093));
#9277=CARTESIAN_POINT('Ctrl Pts',(4.9619552371481,8.2033051832732,-69.8076440049128));
#9278=CARTESIAN_POINT('Ctrl Pts',(4.84737353210574,5.99999999999993,-70.0022474209937));
#9279=CARTESIAN_POINT('Ctrl Pts',(5.95434628461138,5.99999999999976,-68.0771395833567));
#9280=CARTESIAN_POINT('Ctrl Pts',(5.64195423199013,8.19161683866198,-70.249922819652));
#9281=CARTESIAN_POINT('Ctrl Pts',(5.52095572201563,5.99999999999897,-70.4229571273111));
#9282=CARTESIAN_POINT('Ctrl Pts',(6.77034507823848,5.99999999999976,-68.606232644865));
#9283=CARTESIAN_POINT('Ctrl Pts',(6.07167146824097,8.18301541721047,-70.5814843365868));
#9284=CARTESIAN_POINT('Ctrl Pts',(5.94935788369522,5.99999999999975,-70.7404859488671));
#9285=CARTESIAN_POINT('Ctrl Pts',(7.28600576188916,5.99999999999976,-69.0029097959542));
#9286=CARTESIAN_POINT('Ctrl Pts',(6.06845316111809,70.5790021938727,-8.18307981205452));
#9287=CARTESIAN_POINT('Ctrl Pts',(5.9461570612046,70.7381145081864,-6.));
#9288=CARTESIAN_POINT('Ctrl Pts',(7.28214379334171,68.9999401837949,-6.));
#9289=CARTESIAN_POINT('Ctrl Pts',(5.85250470825994,70.412520204687,-8.18739907696574));
#9290=CARTESIAN_POINT('Ctrl Pts',(5.73112901121905,70.5788698227219,-5.99999999999878));
#9291=CARTESIAN_POINT('Ctrl Pts',(7.02300565008836,68.8007627382557,-6.));
#9292=CARTESIAN_POINT('Ctrl Pts',(5.4030400778454,70.094529204984,-8.19572312550303));
#9293=CARTESIAN_POINT('Ctrl Pts',(5.2847582859253,70.2754413258182,-6.00000000000057));
#9294=CARTESIAN_POINT('Ctrl Pts',(6.4836480933326,68.420336950426,-6.));
#9295=CARTESIAN_POINT('Ctrl Pts',(4.70138175653205,69.6800775652252,-8.20673937879446));
#9296=CARTESIAN_POINT('Ctrl Pts',(4.59201175284023,69.8819393154531,-5.99999999999985));
#9297=CARTESIAN_POINT('Ctrl Pts',(5.6416581078604,67.9245467956979,-6.));
#9298=CARTESIAN_POINT('Ctrl Pts',(3.97115974367465,69.3252465860493,-8.21629593855211));
#9299=CARTESIAN_POINT('Ctrl Pts',(3.87398144459366,69.5461824566282,-6.00000000000004));
#9300=CARTESIAN_POINT('Ctrl Pts',(4.7653916924037,67.5001049460443,-6.));
#9301=CARTESIAN_POINT('Ctrl Pts',(3.21394619993446,69.0306051709583,-8.22432109821301));
#9302=CARTESIAN_POINT('Ctrl Pts',(3.13199166924711,69.2682151205242,-5.99999999999999));
#9303=CARTESIAN_POINT('Ctrl Pts',(3.85673543992293,67.1476799730556,-6.));
#9304=CARTESIAN_POINT('Ctrl Pts',(2.42484741772666,68.7962257477066,-8.23076407364235));
#9305=CARTESIAN_POINT('Ctrl Pts',(2.36099569087951,69.04766123426,-6.));
#9306=CARTESIAN_POINT('Ctrl Pts',(2.90981690127157,66.8673480706179,-6.));
#9307=CARTESIAN_POINT('Ctrl Pts',(1.62254651618572,68.6288864435827,-8.23539674526383));
#9308=CARTESIAN_POINT('Ctrl Pts',(1.5788525519209,68.8905076108765,-6.));
#9309=CARTESIAN_POINT('Ctrl Pts',(1.94705581942297,66.6672072720232,-6.));
#9310=CARTESIAN_POINT('Ctrl Pts',(0.809578703168379,68.5281112697337,-8.23819968642438));
#9311=CARTESIAN_POINT('Ctrl Pts',(0.787480259127005,68.795990972133,-6.));
#9312=CARTESIAN_POINT('Ctrl Pts',(0.971494443802027,66.5466812084756,-6.));
#9313=CARTESIAN_POINT('Ctrl Pts',(-0.013029712981914,68.4951024671821,-8.23911996777312));
#9314=CARTESIAN_POINT('Ctrl Pts',(-0.0126728355574548,68.7650536074879,
-6.));
#9315=CARTESIAN_POINT('Ctrl Pts',(-0.0156356555782979,66.50720349905,-6.));
#9316=CARTESIAN_POINT('Ctrl Pts',(-0.82475291689116,68.5297083407777,-8.23815520081018));
#9317=CARTESIAN_POINT('Ctrl Pts',(-0.802248936456917,68.7974884178539,-6.));
#9318=CARTESIAN_POINT('Ctrl Pts',(-0.98970350026936,66.5485912747063,-6.));
#9319=CARTESIAN_POINT('Ctrl Pts',(-1.62999718711769,68.6302910463923,-8.23535781353056));
#9320=CARTESIAN_POINT('Ctrl Pts',(-1.58611884322627,68.8918272865528,-6.));
#9321=CARTESIAN_POINT('Ctrl Pts',(-1.95599662454136,66.668887192006,-6.));
#9322=CARTESIAN_POINT('Ctrl Pts',(-2.42743324168628,68.7969244893687,-8.23074480840111));
#9323=CARTESIAN_POINT('Ctrl Pts',(-2.36352138908597,69.0483185373979,-6.));
#9324=CARTESIAN_POINT('Ctrl Pts',(-2.91291989002306,66.8681837953073,-6.));
#9325=CARTESIAN_POINT('Ctrl Pts',(-3.21786438035412,69.0318882581676,-8.22428592982348));
#9326=CARTESIAN_POINT('Ctrl Pts',(-3.13582126046264,69.2694228660117,-6.));
#9327=CARTESIAN_POINT('Ctrl Pts',(-3.8614372564267,67.1492146449609,-6.));
#9328=CARTESIAN_POINT('Ctrl Pts',(-3.9757652277849,69.3272467095959,-8.21624171003073));
#9329=CARTESIAN_POINT('Ctrl Pts',(-3.87850039141612,69.548071254648,-6.));
#9330=CARTESIAN_POINT('Ctrl Pts',(-4.77091827333531,67.5024973772517,-6.));
#9331=CARTESIAN_POINT('Ctrl Pts',(-4.70599414376018,69.6825677106823,-8.2066727452182));
#9332=CARTESIAN_POINT('Ctrl Pts',(-4.59655713384728,69.8842999100366,-5.99999999999999));
#9333=CARTESIAN_POINT('Ctrl Pts',(-5.64719297253668,67.9275255515984,-6.));
#9334=CARTESIAN_POINT('Ctrl Pts',(-5.4067318828378,70.0969497733373,-8.19565931434823));
#9335=CARTESIAN_POINT('Ctrl Pts',(-5.28841438015195,70.277745403431,-6.00000000000006));
#9336=CARTESIAN_POINT('Ctrl Pts',(-6.48807825931404,68.4232326816432,-6.));
#9337=CARTESIAN_POINT('Ctrl Pts',(-5.85594494885298,70.4150161243228,-8.18733391575405));
#9338=CARTESIAN_POINT('Ctrl Pts',(-5.73454365462802,70.5812501693241,-5.99999999999987));
#9339=CARTESIAN_POINT('Ctrl Pts',(-7.02713393882033,68.80374874693,-6.));
#9340=CARTESIAN_POINT('Ctrl Pts',(-6.07208140606695,70.5818006535869,-8.18300721130884));
#9341=CARTESIAN_POINT('Ctrl Pts',(-5.94976560031573,70.7407881617334,-6.));
#9342=CARTESIAN_POINT('Ctrl Pts',(-7.28649768728034,69.003288234715,-6.));
#9343=CARTESIAN_POINT('Ctrl Pts',(-6.06800331052389,70.5786554091101,8.18308880920814));
#9344=CARTESIAN_POINT('Ctrl Pts',(-5.94570966116718,70.7377831935888,6.));
#9345=CARTESIAN_POINT('Ctrl Pts',(-7.28160397262866,68.9995252938625,6.));
#9346=CARTESIAN_POINT('Ctrl Pts',(-5.85353030598669,70.4133302716269,8.18737811067092));
#9347=CARTESIAN_POINT('Ctrl Pts',(-5.73215330255919,70.5796468161294,5.99999999999929));
#9348=CARTESIAN_POINT('Ctrl Pts',(-7.02423636720416,68.801731905345,6.));
#9349=CARTESIAN_POINT('Ctrl Pts',(-5.41162544279277,70.1002420950884,8.19557272244625));
#9350=CARTESIAN_POINT('Ctrl Pts',(-5.29326845745797,70.2808840380355,6.00000000000033));
#9351=CARTESIAN_POINT('Ctrl Pts',(-6.49395053134197,68.4271713357068,6.));
#9352=CARTESIAN_POINT('Ctrl Pts',(-4.70481487609731,69.68156698975,8.20669879137122));
#9353=CARTESIAN_POINT('Ctrl Pts',(-4.59536063894259,69.8833333373145,5.99999999999991));
#9354=CARTESIAN_POINT('Ctrl Pts',(-5.64577785131928,67.9263283153489,6.));
#9355=CARTESIAN_POINT('Ctrl Pts',(-3.96627549218016,69.3229477280658,8.21635807544407));
#9356=CARTESIAN_POINT('Ctrl Pts',(-3.8691744858435,69.5440067533137,6.00000000000002));
#9357=CARTESIAN_POINT('Ctrl Pts',(-4.75953059061551,67.4973551447454,6.));
#9358=CARTESIAN_POINT('Ctrl Pts',(-3.20911839757511,69.0291784410581,8.22436037712234));
#9359=CARTESIAN_POINT('Ctrl Pts',(-3.12728540351795,69.2668764225387,6.));
#9360=CARTESIAN_POINT('Ctrl Pts',(-3.85094207709032,67.1459735308842,6.));
#9361=CARTESIAN_POINT('Ctrl Pts',(-2.43063423668004,68.7979338632913,8.23071705603037));
#9362=CARTESIAN_POINT('Ctrl Pts',(-2.36665650885803,69.049269954688,6.));
#9363=CARTESIAN_POINT('Ctrl Pts',(-2.916761084016,66.8693910661871,6.));
#9364=CARTESIAN_POINT('Ctrl Pts',(-1.62982756087553,68.6299461600578,8.23536727988032));
#9365=CARTESIAN_POINT('Ctrl Pts',(-1.58593926432988,68.8915009519299,6.));
#9366=CARTESIAN_POINT('Ctrl Pts',(-1.95579307305065,66.6684746840155,6.));
#9367=CARTESIAN_POINT('Ctrl Pts',(-0.812141365160684,68.5283964235732,8.23819173472987));
#9368=CARTESIAN_POINT('Ctrl Pts',(-0.789973040819509,68.7962581236044,6.));
#9369=CARTESIAN_POINT('Ctrl Pts',(-0.974569638192805,66.5470222450721,6.));
#9370=CARTESIAN_POINT('Ctrl Pts',(0.00467372932650424,68.4950285445672,
8.23912206149444));
#9371=CARTESIAN_POINT('Ctrl Pts',(0.00454416602520166,68.7649851030205,
6.));
#9372=CARTESIAN_POINT('Ctrl Pts',(0.00560847519175735,66.5071150964334,
6.));
#9373=CARTESIAN_POINT('Ctrl Pts',(0.828738811659076,68.5296912309094,8.23815554792229));
#9374=CARTESIAN_POINT('Ctrl Pts',(0.80612218834234,68.797469221826,6.));
#9375=CARTESIAN_POINT('Ctrl Pts',(0.994486573991066,66.5485707839574,6.));
#9376=CARTESIAN_POINT('Ctrl Pts',(1.90845066676385,68.6658114852638,8.23437057399169));
#9377=CARTESIAN_POINT('Ctrl Pts',(1.85690343335388,68.9251227747513,6.));
#9378=CARTESIAN_POINT('Ctrl Pts',(2.29014080011569,66.7113694226116,6.));
#9379=CARTESIAN_POINT('Ctrl Pts',(2.95632883002034,68.9305419049585,8.22704718157308));
#9380=CARTESIAN_POINT('Ctrl Pts',(2.87879333312298,69.1735447167021,6.));
#9381=CARTESIAN_POINT('Ctrl Pts',(3.54759459603022,67.0279929531528,6.));
#9382=CARTESIAN_POINT('Ctrl Pts',(3.97967565233726,69.3285749611317,8.21620515776737));
#9383=CARTESIAN_POINT('Ctrl Pts',(3.88231146988333,69.5493124163549,6.00000000000001));
#9384=CARTESIAN_POINT('Ctrl Pts',(4.77561078279477,67.5040860397941,6.));
#9385=CARTESIAN_POINT('Ctrl Pts',(4.96001369761565,69.8069399276529,8.2033245920263));
#9386=CARTESIAN_POINT('Ctrl Pts',(4.84549423190842,70.0015951864197,5.99999999999992));
#9387=CARTESIAN_POINT('Ctrl Pts',(5.9520164371926,68.0762974753181,6.));
#9388=CARTESIAN_POINT('Ctrl Pts',(5.64104467416319,70.2492086476532,8.19163533365013));
#9389=CARTESIAN_POINT('Ctrl Pts',(5.52004559010036,70.4222707745883,6.00000000000035));
#9390=CARTESIAN_POINT('Ctrl Pts',(6.76925360875657,68.6053782094064,6.));
#9391=CARTESIAN_POINT('Ctrl Pts',(6.07181437220709,70.5815946005789,8.18301255673008));
#9392=CARTESIAN_POINT('Ctrl Pts',(5.94950001319883,70.7405912962541,6.));
#9393=CARTESIAN_POINT('Ctrl Pts',(7.28617724664851,69.0030417147821,6.));
#9394=CARTESIAN_POINT('',(0.,0.,0.));
#9395=CARTESIAN_POINT('Origin',(6.,12.,10.3923048454133));
#9396=CARTESIAN_POINT('',(12.,1.60769515458673,-2.07311314789647E-15));
#9397=CARTESIAN_POINT('',(9.,0.,5.19615242270663));
#9398=CARTESIAN_POINT('Ctrl Pts',(11.9999999999992,1.60769515458591,1.42578261298065E-12));
#9399=CARTESIAN_POINT('Ctrl Pts',(10.3923048454129,1.11022302462516E-15,
2.7846096908271));
#9400=CARTESIAN_POINT('Ctrl Pts',(9.,2.73207272303746E-15,5.19615242270663));
#9401=CARTESIAN_POINT('',(12.,10.3923048454133,-3.39099245361938E-15));
#9402=CARTESIAN_POINT('',(12.,10.3923048454133,-3.61640635416958E-15));
#9403=CARTESIAN_POINT('',(9.,12.,5.19615242270663));
#9404=CARTESIAN_POINT('Ctrl Pts',(9.00000000000001,12.,5.19615242270662));
#9405=CARTESIAN_POINT('Ctrl Pts',(10.3923048454129,12.,2.78460969082709));
#9406=CARTESIAN_POINT('Ctrl Pts',(11.9999999999992,10.3923048454141,1.41342337334735E-12));
#9407=CARTESIAN_POINT('',(6.,10.3923048454133,10.3923048454133));
#9408=CARTESIAN_POINT('Ctrl Pts',(6.00000000000083,10.3923048454141,10.3923048454118));
#9409=CARTESIAN_POINT('Ctrl Pts',(7.60769515458707,12.,7.60769515458616));
#9410=CARTESIAN_POINT('Ctrl Pts',(9.00000000000001,12.,5.19615242270662));
#9411=CARTESIAN_POINT('',(6.00000000000079,1.6076951545867,10.3923048454133));
#9412=CARTESIAN_POINT('',(6.,10.3923048454133,10.3923048454133));
#9413=CARTESIAN_POINT('Ctrl Pts',(9.00000000000001,1.09283143764095E-15,
5.19615242270663));
#9414=CARTESIAN_POINT('Ctrl Pts',(7.60769515458714,2.37120928169226E-16,
7.60769515458605));
#9415=CARTESIAN_POINT('Ctrl Pts',(6.00000000000099,1.60769515458575,10.3923048454116));
#9416=CARTESIAN_POINT('Origin',(12.,12.,-3.61640635416958E-15));
#9417=CARTESIAN_POINT('',(6.,1.60769515458673,-10.3923048454133));
#9418=CARTESIAN_POINT('',(9.,0.,-5.19615242270663));
#9419=CARTESIAN_POINT('Ctrl Pts',(6.00000000000082,1.60769515458591,-10.3923048454118));
#9420=CARTESIAN_POINT('Ctrl Pts',(7.60769515458707,5.77315972805081E-15,
-7.60769515458617));
#9421=CARTESIAN_POINT('Ctrl Pts',(9.,4.91773090146743E-15,-5.19615242270664));
#9422=CARTESIAN_POINT('',(6.00000000000009,10.3923048454133,-10.3923048454133));
#9423=CARTESIAN_POINT('',(6.,10.3923048454133,-10.3923048454133));
#9424=CARTESIAN_POINT('',(9.00000000000001,12.,-5.19615242270663));
#9425=CARTESIAN_POINT('Ctrl Pts',(9.00000000000001,12.,-5.19615242270662));
#9426=CARTESIAN_POINT('Ctrl Pts',(7.60769515458708,12.,-7.60769515458614));
#9427=CARTESIAN_POINT('Ctrl Pts',(6.00000000000086,10.3923048454141,-10.3923048454118));
#9428=CARTESIAN_POINT('Ctrl Pts',(11.9999999999992,10.3923048454141,-1.43697061821777E-12));
#9429=CARTESIAN_POINT('Ctrl Pts',(10.3923048454129,12.,-2.7846096908271));
#9430=CARTESIAN_POINT('Ctrl Pts',(9.00000000000001,12.,-5.19615242270662));
#9431=CARTESIAN_POINT('Ctrl Pts',(9.,4.64453360997405E-15,-5.19615242270664));
#9432=CARTESIAN_POINT('Ctrl Pts',(10.3923048454129,4.94022392384109E-15,
-2.78460969082711));
#9433=CARTESIAN_POINT('Ctrl Pts',(11.9999999999992,1.60769515458591,-1.43226116924369E-12));
#9434=CARTESIAN_POINT('Origin',(6.,12.,-10.3923048454133));
#9435=CARTESIAN_POINT('',(-6.,1.60769515458673,-10.3923048454133));
#9436=CARTESIAN_POINT('',(0.,0.,-10.3923048454133));
#9437=CARTESIAN_POINT('Ctrl Pts',(-5.99999999999835,1.60769515458591,-10.3923048454133));
#9438=CARTESIAN_POINT('Ctrl Pts',(-2.78460969082587,6.43929354282591E-15,
-10.3923048454133));
#9439=CARTESIAN_POINT('Ctrl Pts',(-2.18565828465779E-15,6.55697485397336E-15,
-10.3923048454133));
#9440=CARTESIAN_POINT('',(-6.,10.3923048454133,-10.3923048454133));
#9441=CARTESIAN_POINT('',(-6.,10.3923048454133,-10.3923048454133));
#9442=CARTESIAN_POINT('',(0.,12.,-10.3923048454133));
#9443=CARTESIAN_POINT('Ctrl Pts',(2.62278997768546E-14,12.,-10.3923048454133));
#9444=CARTESIAN_POINT('Ctrl Pts',(-2.78460969082585,12.,-10.3923048454133));
#9445=CARTESIAN_POINT('Ctrl Pts',(-5.99999999999834,10.3923048454141,-10.3923048454133));
#9446=CARTESIAN_POINT('Ctrl Pts',(5.99999999999843,10.3923048454141,-10.3923048454133));
#9447=CARTESIAN_POINT('Ctrl Pts',(2.78460969082591,12.,-10.3923048454133));
#9448=CARTESIAN_POINT('Ctrl Pts',(2.62278997768546E-14,12.,-10.3923048454133));
#9449=CARTESIAN_POINT('Ctrl Pts',(-1.52996401269733E-14,3.82491003174334E-15,
-10.3923048454133));
#9450=CARTESIAN_POINT('Ctrl Pts',(2.78460969082586,6.26139843732123E-17,
-10.3923048454133));
#9451=CARTESIAN_POINT('Ctrl Pts',(5.99999999999836,1.60769515458591,-10.3923048454133));
#9452=CARTESIAN_POINT('Origin',(-6.,12.,-10.3923048454133));
#9453=CARTESIAN_POINT('',(-12.,1.60769515458673,-1.44959860074153E-16));
#9454=CARTESIAN_POINT('',(-9.,0.,-5.19615242270663));
#9455=CARTESIAN_POINT('Ctrl Pts',(-11.9999999999992,1.60769515458591,-1.42813733240754E-12));
#9456=CARTESIAN_POINT('Ctrl Pts',(-10.3923048454129,-6.66133814775094E-16,
-2.78460969082711));
#9457=CARTESIAN_POINT('Ctrl Pts',(-9.,1.63924363382248E-15,-5.19615242270664));
#9458=CARTESIAN_POINT('',(-12.,10.3923048454133,-1.19184216575765E-16));
#9459=CARTESIAN_POINT('',(-12.,10.3923048454133,1.23259516440783E-29));
#9460=CARTESIAN_POINT('',(-9.00000000000001,12.,-5.19615242270663));
#9461=CARTESIAN_POINT('Ctrl Pts',(-9.,12.,-5.19615242270663));
#9462=CARTESIAN_POINT('Ctrl Pts',(-10.3923048454129,12.,-2.7846096908271));
#9463=CARTESIAN_POINT('Ctrl Pts',(-11.9999999999992,10.3923048454141,-1.4246083146608E-12));
#9464=CARTESIAN_POINT('Ctrl Pts',(-6.00000000000082,10.3923048454141,-10.3923048454118));
#9465=CARTESIAN_POINT('Ctrl Pts',(-7.60769515458707,12.,-7.60769515458616));
#9466=CARTESIAN_POINT('Ctrl Pts',(-9.,12.,-5.19615242270663));
#9467=CARTESIAN_POINT('Ctrl Pts',(-9.00000000000001,6.55698862584572E-15,
-5.19615242270663));
#9468=CARTESIAN_POINT('Ctrl Pts',(-7.60769515458707,6.21840847038348E-15,
-7.60769515458617));
#9469=CARTESIAN_POINT('Ctrl Pts',(-6.00000000000082,1.60769515458592,-10.3923048454119));
#9470=CARTESIAN_POINT('Origin',(-12.,12.,1.23259516440783E-29));
#9471=CARTESIAN_POINT('',(-6.,1.60769515458673,10.3923048454133));
#9472=CARTESIAN_POINT('',(-9.,0.,5.19615242270663));
#9473=CARTESIAN_POINT('Ctrl Pts',(-6.00000000000082,1.60769515458591,10.3923048454118));
#9474=CARTESIAN_POINT('Ctrl Pts',(-7.60769515458707,-1.77635683940025E-15,
7.60769515458616));
#9475=CARTESIAN_POINT('Ctrl Pts',(-9.00000000000001,4.91773090146746E-15,
5.19615242270662));
#9476=CARTESIAN_POINT('',(-6.0000000000001,10.3923048454133,10.3923048454133));
#9477=CARTESIAN_POINT('',(-6.,10.3923048454133,10.3923048454133));
#9478=CARTESIAN_POINT('',(-9.00000000000001,12.,5.19615242270663));
#9479=CARTESIAN_POINT('Ctrl Pts',(-9.,12.,5.19615242270663));
#9480=CARTESIAN_POINT('Ctrl Pts',(-7.60769515458708,12.,7.60769515458614));
#9481=CARTESIAN_POINT('Ctrl Pts',(-6.00000000000085,10.3923048454141,10.3923048454118));
#9482=CARTESIAN_POINT('Ctrl Pts',(-11.9999999999992,10.3923048454141,1.42931776363488E-12));
#9483=CARTESIAN_POINT('Ctrl Pts',(-10.3923048454129,12.,2.7846096908271));
#9484=CARTESIAN_POINT('Ctrl Pts',(-9.,12.,5.19615242270663));
#9485=CARTESIAN_POINT('Ctrl Pts',(-9.00000000000001,5.46415718820513E-16,
5.19615242270661));
#9486=CARTESIAN_POINT('Ctrl Pts',(-10.3923048454129,8.17530773838345E-15,
2.78460969082708));
#9487=CARTESIAN_POINT('Ctrl Pts',(-11.9999999999992,1.60769515458592,1.41165732998206E-12));
#9488=CARTESIAN_POINT('Origin',(-6.,12.,10.3923048454133));
#9489=CARTESIAN_POINT('',(-1.50231459873716E-15,0.,10.3923048454133));
#9490=CARTESIAN_POINT('Ctrl Pts',(5.99999999999897,1.60769515458622,10.3923048454133));
#9491=CARTESIAN_POINT('Ctrl Pts',(2.78460969082611,3.10862446895044E-15,
10.3923048454133));
#9492=CARTESIAN_POINT('Ctrl Pts',(-1.09282914232889E-15,3.00528014140446E-15,
10.3923048454133));
#9493=CARTESIAN_POINT('',(-1.73472347597681E-15,12.,10.3923048454133));
#9494=CARTESIAN_POINT('Ctrl Pts',(-2.34958268834322E-14,12.,10.3923048454133));
#9495=CARTESIAN_POINT('Ctrl Pts',(2.78460969082586,12.,10.3923048454133));
#9496=CARTESIAN_POINT('Ctrl Pts',(5.99999999999836,10.3923048454141,10.3923048454133));
#9497=CARTESIAN_POINT('Ctrl Pts',(-5.99999999999843,10.3923048454141,10.3923048454133));
#9498=CARTESIAN_POINT('Ctrl Pts',(-2.78460969082591,12.,10.3923048454133));
#9499=CARTESIAN_POINT('Ctrl Pts',(-2.34958268834322E-14,12.,10.3923048454133));
#9500=CARTESIAN_POINT('Ctrl Pts',(6.55698862584571E-15,8.19623578230717E-16,
10.3923048454133));
#9501=CARTESIAN_POINT('Ctrl Pts',(-2.78460969082587,-1.06903685822888E-15,
10.3923048454133));
#9502=CARTESIAN_POINT('Ctrl Pts',(-5.99999999999837,1.60769515458591,10.3923048454133));
#9503=CARTESIAN_POINT('Origin',(0.,0.,0.));
#9504=CARTESIAN_POINT('Origin',(0.,0.,0.));
#9505=CARTESIAN_POINT('Origin',(0.,0.,0.));
#9506=CARTESIAN_POINT('Origin',(0.,0.,0.));
#9507=CARTESIAN_POINT('Origin',(0.,0.,0.));
#9508=CARTESIAN_POINT('Origin',(0.,0.,0.));
#9509=CARTESIAN_POINT('Origin',(0.,0.,0.));
#9510=CARTESIAN_POINT('',(0.,0.,6.));
#9511=CARTESIAN_POINT('Origin',(0.,0.,0.));
#9512=CARTESIAN_POINT('Origin',(0.,12.,0.));
#9513=CARTESIAN_POINT('Origin',(0.,12.,0.));
#9514=CARTESIAN_POINT('Origin',(0.,12.,0.));
#9515=CARTESIAN_POINT('Origin',(0.,12.,0.));
#9516=CARTESIAN_POINT('Origin',(0.,12.,0.));
#9517=CARTESIAN_POINT('Origin',(0.,12.,0.));
#9518=CARTESIAN_POINT('Origin',(0.,12.,0.));
#9519=CARTESIAN_POINT('',(0.,12.,6.));
#9520=CARTESIAN_POINT('Origin',(0.,12.,0.));
#9521=CARTESIAN_POINT('Origin',(0.,12.,0.));
#9522=CARTESIAN_POINT('',(-7.34788079488412E-16,12.,6.));
#9523=CARTESIAN_POINT('Origin',(0.,12.,0.));
#9524=CARTESIAN_POINT('Origin',(0.,12.,0.));
#9525=CARTESIAN_POINT('Origin',(0.,12.,0.));
#9526=CARTESIAN_POINT('Origin',(0.,12.,0.));
#9527=CARTESIAN_POINT('Origin',(0.,12.,0.));
#9528=CARTESIAN_POINT('Origin',(0.,12.,0.));
#9529=CARTESIAN_POINT('Origin',(0.,0.,0.));
#9530=CARTESIAN_POINT('Origin',(0.,0.,0.));
#9531=CARTESIAN_POINT('Origin',(0.,0.,0.));
#9532=CARTESIAN_POINT('Origin',(0.,0.,0.));
#9533=CARTESIAN_POINT('Origin',(0.,0.,0.));
#9534=CARTESIAN_POINT('Origin',(0.,0.,0.));
#9535=CARTESIAN_POINT('',(0.,0.,0.));
#9536=CARTESIAN_POINT('Origin',(6.00000000000001,41.,10.3923048454133));
#9537=CARTESIAN_POINT('',(6.00000000000001,39.3923048454133,10.3923048454133));
#9538=CARTESIAN_POINT('',(9.00000000000001,41.,5.19615242270664));
#9539=CARTESIAN_POINT('Ctrl Pts',(6.00000000000003,39.3923048454133,10.3923048454132));
#9540=CARTESIAN_POINT('Ctrl Pts',(7.60769515458675,41.,7.60769515458673));
#9541=CARTESIAN_POINT('Ctrl Pts',(9.00000000000001,41.,5.19615242270663));
#9542=CARTESIAN_POINT('',(6.00000000000001,32.,10.3923048454133));
#9543=CARTESIAN_POINT('',(6.00000000000001,39.3923048454133,10.3923048454133));
#9544=CARTESIAN_POINT('',(12.,32.,1.67859117701527E-16));
#9545=CARTESIAN_POINT('',(6.00000000000001,32.,10.3923048454133));
#9546=CARTESIAN_POINT('',(12.,39.3923048454133,9.21294328526909E-16));
#9547=CARTESIAN_POINT('',(12.,39.3923048454133,1.67859117701527E-16));
#9548=CARTESIAN_POINT('Ctrl Pts',(9.00000000000001,41.,5.19615242270663));
#9549=CARTESIAN_POINT('Ctrl Pts',(10.3923048454133,41.,2.78460969082656));
#9550=CARTESIAN_POINT('Ctrl Pts',(12.,39.3923048454133,7.39725942272692E-14));
#9551=CARTESIAN_POINT('Origin',(12.,41.,1.67859117701527E-16));
#9552=CARTESIAN_POINT('',(9.00000000000001,41.,-5.19615242270664));
#9553=CARTESIAN_POINT('Ctrl Pts',(12.,39.3923048454133,-3.52096627544644E-14));
#9554=CARTESIAN_POINT('Ctrl Pts',(10.3923048454133,41.,-2.78460969082656));
#9555=CARTESIAN_POINT('Ctrl Pts',(8.99999999999999,41.,-5.19615242270666));
#9556=CARTESIAN_POINT('',(6.00000000000001,32.,-10.3923048454133));
#9557=CARTESIAN_POINT('',(12.,32.,1.67859117701527E-16));
#9558=CARTESIAN_POINT('',(6.00000000000001,39.3923048454133,-10.3923048454133));
#9559=CARTESIAN_POINT('',(6.00000000000001,39.3923048454133,-10.3923048454133));
#9560=CARTESIAN_POINT('Ctrl Pts',(8.99999999999999,41.,-5.19615242270666));
#9561=CARTESIAN_POINT('Ctrl Pts',(7.60769515458674,41.,-7.60769515458675));
#9562=CARTESIAN_POINT('Ctrl Pts',(6.00000000000002,39.3923048454133,-10.3923048454133));
#9563=CARTESIAN_POINT('Origin',(6.00000000000001,41.,-10.3923048454133));
#9564=CARTESIAN_POINT('',(1.50231459873716E-15,41.,-10.3923048454133));
#9565=CARTESIAN_POINT('Ctrl Pts',(5.99999999999996,39.3923048454133,-10.3923048454133));
#9566=CARTESIAN_POINT('Ctrl Pts',(2.78460969082653,41.,-10.3923048454133));
#9567=CARTESIAN_POINT('Ctrl Pts',(3.47805489344055E-14,41.,-10.3923048454133));
#9568=CARTESIAN_POINT('',(-6.,32.,-10.3923048454133));
#9569=CARTESIAN_POINT('',(6.00000000000001,32.,-10.3923048454133));
#9570=CARTESIAN_POINT('',(-6.,39.3923048454133,-10.3923048454133));
#9571=CARTESIAN_POINT('',(-6.,39.3923048454133,-10.3923048454133));
#9572=CARTESIAN_POINT('Ctrl Pts',(3.47805489344055E-14,41.,-10.3923048454133));
#9573=CARTESIAN_POINT('Ctrl Pts',(-2.78460969082651,41.,-10.3923048454133));
#9574=CARTESIAN_POINT('Ctrl Pts',(-6.00000000000001,39.3923048454133,-10.3923048454133));
#9575=CARTESIAN_POINT('Origin',(-6.,41.,-10.3923048454133));
#9576=CARTESIAN_POINT('',(-9.00000000000001,41.,-5.19615242270664));
#9577=CARTESIAN_POINT('Ctrl Pts',(-6.00000000000002,39.3923048454133,-10.3923048454132));
#9578=CARTESIAN_POINT('Ctrl Pts',(-7.60769515458675,41.,-7.60769515458673));
#9579=CARTESIAN_POINT('Ctrl Pts',(-9.00000000000001,41.,-5.19615242270663));
#9580=CARTESIAN_POINT('',(-12.,32.,2.18193936935029E-15));
#9581=CARTESIAN_POINT('',(-6.,32.,-10.3923048454133));
#9582=CARTESIAN_POINT('',(-12.,39.3923048454133,7.91126054510164E-16));
#9583=CARTESIAN_POINT('',(-12.,39.3923048454133,2.18193936935029E-15));
#9584=CARTESIAN_POINT('Ctrl Pts',(-9.00000000000001,41.,-5.19615242270663));
#9585=CARTESIAN_POINT('Ctrl Pts',(-10.3923048454133,41.,-2.78460969082655));
#9586=CARTESIAN_POINT('Ctrl Pts',(-12.,39.3923048454133,-5.42681040619267E-14));
#9587=CARTESIAN_POINT('Origin',(-12.,41.,2.18193936935029E-15));
#9588=CARTESIAN_POINT('',(-9.00000000000001,41.,5.19615242270664));
#9589=CARTESIAN_POINT('Ctrl Pts',(-12.,39.3923048454133,3.45636138965843E-14));
#9590=CARTESIAN_POINT('Ctrl Pts',(-10.3923048454133,41.,2.78460969082656));
#9591=CARTESIAN_POINT('Ctrl Pts',(-8.99999999999999,41.,5.19615242270666));
#9592=CARTESIAN_POINT('',(-6.,32.,10.3923048454133));
#9593=CARTESIAN_POINT('',(-12.,32.,2.18193936935029E-15));
#9594=CARTESIAN_POINT('',(-6.,39.3923048454133,10.3923048454133));
#9595=CARTESIAN_POINT('',(-6.,39.3923048454133,10.3923048454133));
#9596=CARTESIAN_POINT('Ctrl Pts',(-8.99999999999999,41.,5.19615242270666));
#9597=CARTESIAN_POINT('Ctrl Pts',(-7.60769515458674,41.,7.60769515458673));
#9598=CARTESIAN_POINT('Ctrl Pts',(-6.00000000000003,39.3923048454133,10.3923048454132));
#9599=CARTESIAN_POINT('Origin',(-6.,41.,10.3923048454133));
#9600=CARTESIAN_POINT('',(0.,41.,10.3923048454133));
#9601=CARTESIAN_POINT('Ctrl Pts',(-5.99999999999996,39.3923048454133,10.3923048454133));
#9602=CARTESIAN_POINT('Ctrl Pts',(-2.7846096908265,41.,10.3923048454133));
#9603=CARTESIAN_POINT('Ctrl Pts',(1.67906098304027E-14,41.,10.3923048454133));
#9604=CARTESIAN_POINT('',(-6.,32.,10.3923048454133));
#9605=CARTESIAN_POINT('Ctrl Pts',(1.67906098304027E-14,41.,10.3923048454133));
#9606=CARTESIAN_POINT('Ctrl Pts',(2.78460969082651,41.,10.3923048454133));
#9607=CARTESIAN_POINT('Ctrl Pts',(5.99999999999992,39.3923048454133,10.3923048454133));
#9608=CARTESIAN_POINT('Origin',(0.,32.,0.));
#9609=CARTESIAN_POINT('',(0.,0.,6.));
#9610=CARTESIAN_POINT('Origin',(0.,0.,0.));
#9611=CARTESIAN_POINT('',(0.,32.,6.));
#9612=CARTESIAN_POINT('',(-7.34788079488412E-16,32.,6.));
#9613=CARTESIAN_POINT('Origin',(0.,32.,0.));
#9614=CARTESIAN_POINT('Origin',(0.,0.,0.));
#9615=CARTESIAN_POINT('Origin',(0.,32.,0.));
#9616=CARTESIAN_POINT('Origin',(0.,41.,0.));
#9617=CARTESIAN_POINT('Origin',(0.,41.,0.));
#9618=CARTESIAN_POINT('Origin',(0.,41.,0.));
#9619=CARTESIAN_POINT('Origin',(0.,41.,0.));
#9620=CARTESIAN_POINT('Origin',(0.,41.,0.));
#9621=CARTESIAN_POINT('Origin',(0.,41.,0.));
#9622=CARTESIAN_POINT('Origin',(0.,41.,0.));
#9623=CARTESIAN_POINT('Origin',(0.,41.,0.));
#9624=CARTESIAN_POINT('Origin',(0.,41.,0.));
#9625=CARTESIAN_POINT('Origin',(0.,41.,0.));
#9626=CARTESIAN_POINT('Origin',(0.,41.,0.));
#9627=CARTESIAN_POINT('Origin',(0.,41.,0.));
#9628=CARTESIAN_POINT('Origin',(0.,41.,0.));
#9629=CARTESIAN_POINT('',(735.744941914433,952.769965467177,1363.37377366647));
#9630=CARTESIAN_POINT('',(735.744941914436,948.769965467175,1363.37377366647));
#9631=CARTESIAN_POINT('',(735.74494191443,956.769965467177,1363.37377366647));
#9632=CARTESIAN_POINT('',(735.744941914436,960.769965467175,1363.37377366647));
#9633=CARTESIAN_POINT('',(735.744941914428,966.769965467177,1349.37377366648));
#9634=CARTESIAN_POINT('',(735.744941914423,1028.76996546717,1363.37377366648));
#9635=CARTESIAN_POINT('',(735.744941914433,1062.76996546717,1363.37377366648));
#9636=CARTESIAN_POINT('',(735.744941914433,1048.76996546717,1363.37377366648));
#9637=CARTESIAN_POINT('',(735.744941914427,1182.76996546718,1363.37377366647));
#9638=CARTESIAN_POINT('',(735.744941914436,1192.76996546717,1363.37377366647));
#9639=CARTESIAN_POINT('',(665.744941914433,1016.76996546717,1363.37377366648));
#9640=CARTESIAN_POINT('',(735.744941914429,1016.76996546717,1293.37377366647));
#9641=CARTESIAN_POINT('',(805.744941914432,1016.76996546717,1363.37377366647));
#9642=CARTESIAN_POINT('',(735.744941914435,1016.76996546717,1433.37377366647));
#9643=UNCERTAINTY_MEASURE_WITH_UNIT(LENGTH_MEASURE(0.01),#9669,
'DISTANCE_ACCURACY_VALUE',
'Maximum model space distance between geometric entities at asserted c
onnectivities');
#9644=UNCERTAINTY_MEASURE_WITH_UNIT(LENGTH_MEASURE(0.01),#9669,
'DISTANCE_ACCURACY_VALUE',
'Maximum model space distance between geometric entities at asserted c
onnectivities');
#9645=UNCERTAINTY_MEASURE_WITH_UNIT(LENGTH_MEASURE(0.01),#9669,
'DISTANCE_ACCURACY_VALUE',
'Maximum model space distance between geometric entities at asserted c
onnectivities');
#9646=UNCERTAINTY_MEASURE_WITH_UNIT(LENGTH_MEASURE(0.01),#9669,
'DISTANCE_ACCURACY_VALUE',
'Maximum model space distance between geometric entities at asserted c
onnectivities');
#9647=UNCERTAINTY_MEASURE_WITH_UNIT(LENGTH_MEASURE(0.01),#9669,
'DISTANCE_ACCURACY_VALUE',
'Maximum model space distance between geometric entities at asserted c
onnectivities');
#9648=UNCERTAINTY_MEASURE_WITH_UNIT(LENGTH_MEASURE(0.01),#9669,
'DISTANCE_ACCURACY_VALUE',
'Maximum model space distance between geometric entities at asserted c
onnectivities');
#9649=UNCERTAINTY_MEASURE_WITH_UNIT(LENGTH_MEASURE(0.01),#9669,
'DISTANCE_ACCURACY_VALUE',
'Maximum model space distance between geometric entities at asserted c
onnectivities');
#9650=UNCERTAINTY_MEASURE_WITH_UNIT(LENGTH_MEASURE(0.01),#9669,
'DISTANCE_ACCURACY_VALUE',
'Maximum model space distance between geometric entities at asserted c
onnectivities');
#9651=UNCERTAINTY_MEASURE_WITH_UNIT(LENGTH_MEASURE(0.01),#9669,
'DISTANCE_ACCURACY_VALUE',
'Maximum model space distance between geometric entities at asserted c
onnectivities');
#9652=UNCERTAINTY_MEASURE_WITH_UNIT(LENGTH_MEASURE(0.01),#9669,
'DISTANCE_ACCURACY_VALUE',
'Maximum model space distance between geometric entities at asserted c
onnectivities');
#9653=UNCERTAINTY_MEASURE_WITH_UNIT(LENGTH_MEASURE(0.01),#9669,
'DISTANCE_ACCURACY_VALUE',
'Maximum model space distance between geometric entities at asserted c
onnectivities');
#9654=UNCERTAINTY_MEASURE_WITH_UNIT(LENGTH_MEASURE(0.01),#9669,
'DISTANCE_ACCURACY_VALUE',
'Maximum model space distance between geometric entities at asserted c
onnectivities');
#9655=UNCERTAINTY_MEASURE_WITH_UNIT(LENGTH_MEASURE(0.01),#9669,
'DISTANCE_ACCURACY_VALUE',
'Maximum model space distance between geometric entities at asserted c
onnectivities');
#9656=(
GEOMETRIC_REPRESENTATION_CONTEXT(3)
GLOBAL_UNCERTAINTY_ASSIGNED_CONTEXT((#9643))
GLOBAL_UNIT_ASSIGNED_CONTEXT((#9669,#9671,#9672))
REPRESENTATION_CONTEXT('','3D')
);
#9657=(
GEOMETRIC_REPRESENTATION_CONTEXT(3)
GLOBAL_UNCERTAINTY_ASSIGNED_CONTEXT((#9644))
GLOBAL_UNIT_ASSIGNED_CONTEXT((#9669,#9671,#9672))
REPRESENTATION_CONTEXT('','3D')
);
#9658=(
GEOMETRIC_REPRESENTATION_CONTEXT(3)
GLOBAL_UNCERTAINTY_ASSIGNED_CONTEXT((#9645))
GLOBAL_UNIT_ASSIGNED_CONTEXT((#9669,#9671,#9672))
REPRESENTATION_CONTEXT('','3D')
);
#9659=(
GEOMETRIC_REPRESENTATION_CONTEXT(3)
GLOBAL_UNCERTAINTY_ASSIGNED_CONTEXT((#9646))
GLOBAL_UNIT_ASSIGNED_CONTEXT((#9669,#9671,#9672))
REPRESENTATION_CONTEXT('','3D')
);
#9660=(
GEOMETRIC_REPRESENTATION_CONTEXT(3)
GLOBAL_UNCERTAINTY_ASSIGNED_CONTEXT((#9647))
GLOBAL_UNIT_ASSIGNED_CONTEXT((#9669,#9671,#9672))
REPRESENTATION_CONTEXT('','3D')
);
#9661=(
GEOMETRIC_REPRESENTATION_CONTEXT(3)
GLOBAL_UNCERTAINTY_ASSIGNED_CONTEXT((#9648))
GLOBAL_UNIT_ASSIGNED_CONTEXT((#9669,#9671,#9672))
REPRESENTATION_CONTEXT('','3D')
);
#9662=(
GEOMETRIC_REPRESENTATION_CONTEXT(3)
GLOBAL_UNCERTAINTY_ASSIGNED_CONTEXT((#9649))
GLOBAL_UNIT_ASSIGNED_CONTEXT((#9669,#9671,#9672))
REPRESENTATION_CONTEXT('','3D')
);
#9663=(
GEOMETRIC_REPRESENTATION_CONTEXT(3)
GLOBAL_UNCERTAINTY_ASSIGNED_CONTEXT((#9650))
GLOBAL_UNIT_ASSIGNED_CONTEXT((#9669,#9671,#9672))
REPRESENTATION_CONTEXT('','3D')
);
#9664=(
GEOMETRIC_REPRESENTATION_CONTEXT(3)
GLOBAL_UNCERTAINTY_ASSIGNED_CONTEXT((#9651))
GLOBAL_UNIT_ASSIGNED_CONTEXT((#9669,#9671,#9672))
REPRESENTATION_CONTEXT('','3D')
);
#9665=(
GEOMETRIC_REPRESENTATION_CONTEXT(3)
GLOBAL_UNCERTAINTY_ASSIGNED_CONTEXT((#9652))
GLOBAL_UNIT_ASSIGNED_CONTEXT((#9669,#9671,#9672))
REPRESENTATION_CONTEXT('','3D')
);
#9666=(
GEOMETRIC_REPRESENTATION_CONTEXT(3)
GLOBAL_UNCERTAINTY_ASSIGNED_CONTEXT((#9653))
GLOBAL_UNIT_ASSIGNED_CONTEXT((#9669,#9671,#9672))
REPRESENTATION_CONTEXT('','3D')
);
#9667=(
GEOMETRIC_REPRESENTATION_CONTEXT(3)
GLOBAL_UNCERTAINTY_ASSIGNED_CONTEXT((#9654))
GLOBAL_UNIT_ASSIGNED_CONTEXT((#9669,#9671,#9672))
REPRESENTATION_CONTEXT('','3D')
);
#9668=(
GEOMETRIC_REPRESENTATION_CONTEXT(3)
GLOBAL_UNCERTAINTY_ASSIGNED_CONTEXT((#9655))
GLOBAL_UNIT_ASSIGNED_CONTEXT((#9669,#9671,#9672))
REPRESENTATION_CONTEXT('','3D')
);
#9669=(
LENGTH_UNIT()
NAMED_UNIT(*)
SI_UNIT(.MILLI.,.METRE.)
);
#9670=(
LENGTH_UNIT()
NAMED_UNIT(*)
SI_UNIT($,.METRE.)
);
#9671=(
NAMED_UNIT(*)
PLANE_ANGLE_UNIT()
SI_UNIT($,.RADIAN.)
);
#9672=(
NAMED_UNIT(*)
SI_UNIT($,.STERADIAN.)
SOLID_ANGLE_UNIT()
);
#9673=SHAPE_DEFINITION_REPRESENTATION(#9685,#9711);
#9674=SHAPE_DEFINITION_REPRESENTATION(#9686,#9712);
#9675=SHAPE_DEFINITION_REPRESENTATION(#9687,#9713);
#9676=SHAPE_DEFINITION_REPRESENTATION(#9688,#9714);
#9677=SHAPE_DEFINITION_REPRESENTATION(#9689,#9715);
#9678=SHAPE_DEFINITION_REPRESENTATION(#9690,#9716);
#9679=SHAPE_DEFINITION_REPRESENTATION(#9691,#9717);
#9680=SHAPE_DEFINITION_REPRESENTATION(#9692,#9718);
#9681=SHAPE_DEFINITION_REPRESENTATION(#9693,#9719);
#9682=SHAPE_DEFINITION_REPRESENTATION(#9694,#9720);
#9683=SHAPE_DEFINITION_REPRESENTATION(#9695,#9721);
#9684=SHAPE_DEFINITION_REPRESENTATION(#9696,#9722);
#9685=PRODUCT_DEFINITION_SHAPE('',$,#9724);
#9686=PRODUCT_DEFINITION_SHAPE('',$,#9725);
#9687=PRODUCT_DEFINITION_SHAPE('',$,#9726);
#9688=PRODUCT_DEFINITION_SHAPE('',$,#9727);
#9689=PRODUCT_DEFINITION_SHAPE('',$,#9728);
#9690=PRODUCT_DEFINITION_SHAPE('',$,#9729);
#9691=PRODUCT_DEFINITION_SHAPE('',$,#9730);
#9692=PRODUCT_DEFINITION_SHAPE('',$,#9731);
#9693=PRODUCT_DEFINITION_SHAPE('',$,#9732);
#9694=PRODUCT_DEFINITION_SHAPE('',$,#9733);
#9695=PRODUCT_DEFINITION_SHAPE('',$,#9734);
#9696=PRODUCT_DEFINITION_SHAPE('',$,#9735);
#9697=PRODUCT_DEFINITION_SHAPE($,$,#53);
#9698=PRODUCT_DEFINITION_SHAPE($,$,#54);
#9699=PRODUCT_DEFINITION_SHAPE($,$,#55);
#9700=PRODUCT_DEFINITION_SHAPE($,$,#56);
#9701=PRODUCT_DEFINITION_SHAPE($,$,#57);
#9702=PRODUCT_DEFINITION_SHAPE($,$,#58);
#9703=PRODUCT_DEFINITION_SHAPE($,$,#59);
#9704=PRODUCT_DEFINITION_SHAPE($,$,#60);
#9705=PRODUCT_DEFINITION_SHAPE($,$,#61);
#9706=PRODUCT_DEFINITION_SHAPE($,$,#62);
#9707=PRODUCT_DEFINITION_SHAPE($,$,#63);
#9708=PRODUCT_DEFINITION_SHAPE($,$,#64);
#9709=PRODUCT_DEFINITION_SHAPE($,$,#65);
#9710=PRODUCT_DEFINITION_SHAPE($,$,#66);
#9711=SHAPE_REPRESENTATION('',(#4014,#4455,#4456,#4457,#4458,#4459,#4460,
#4461,#4462,#4463,#4464,#4465,#4466,#4467,#4468),#9656);
#9712=SHAPE_REPRESENTATION('',(#4015),#9657);
#9713=SHAPE_REPRESENTATION('',(#4135),#9658);
#9714=SHAPE_REPRESENTATION('',(#4194),#9659);
#9715=SHAPE_REPRESENTATION('',(#4223),#9660);
#9716=SHAPE_REPRESENTATION('',(#4234),#9661);
#9717=SHAPE_REPRESENTATION('',(#4240),#9662);
#9718=SHAPE_REPRESENTATION('',(#4279),#9663);
#9719=SHAPE_REPRESENTATION('',(#4292),#9664);
#9720=SHAPE_REPRESENTATION('',(#4326),#9665);
#9721=SHAPE_REPRESENTATION('',(#4394),#9666);
#9722=SHAPE_REPRESENTATION('',(#4430),#9667);
#9723=PRODUCT_DEFINITION_CONTEXT('part definition',#9761,'design');
#9724=PRODUCT_DEFINITION('2026-10-04-08-13-48-879','MAS-611',#9736,
#9723);
#9725=PRODUCT_DEFINITION('2026-10-04-08-13-48-880','VALVE_BODY',#9737,#9723);
#9726=PRODUCT_DEFINITION('2026-10-04-08-13-48-881','VALVE_DISC',#9738,#9723);
#9727=PRODUCT_DEFINITION('2026-10-04-08-13-48-882','SPINDLE',#9739,#9723);
#9728=PRODUCT_DEFINITION('2026-10-04-08-13-48-883','SPINDLE_COLLAR',#9740,
#9723);
#9729=PRODUCT_DEFINITION('2026-10-04-08-13-48-884','RETAINING_PIN',#9741,
#9723);
#9730=PRODUCT_DEFINITION('2026-10-04-08-13-48-885','BONNET_COVER',#9742,
#9723);
#9731=PRODUCT_DEFINITION('2026-10-04-08-13-48-886','PACKING_GLAND',#9743,
#9723);
#9732=PRODUCT_DEFINITION('2026-10-04-08-13-48-887','GLAND_NUT',#9744,#9723);
#9733=PRODUCT_DEFINITION('2026-10-04-08-13-48-888','HANDWHEEL',#9745,#9723);
#9734=PRODUCT_DEFINITION('2026-10-04-08-13-48-889','NUT',#9746,#9723);
#9735=PRODUCT_DEFINITION('2026-10-04-08-13-48-890','BOLT',#9747,#9723);
#9736=PRODUCT_DEFINITION_FORMATION('',$,#9763);
#9737=PRODUCT_DEFINITION_FORMATION('',$,#9764);
#9738=PRODUCT_DEFINITION_FORMATION('',$,#9765);
#9739=PRODUCT_DEFINITION_FORMATION('',$,#9766);
#9740=PRODUCT_DEFINITION_FORMATION('',$,#9767);
#9741=PRODUCT_DEFINITION_FORMATION('',$,#9768);
#9742=PRODUCT_DEFINITION_FORMATION('',$,#9769);
#9743=PRODUCT_DEFINITION_FORMATION('',$,#9770);
#9744=PRODUCT_DEFINITION_FORMATION('',$,#9771);
#9745=PRODUCT_DEFINITION_FORMATION('',$,#9772);
#9746=PRODUCT_DEFINITION_FORMATION('',$,#9773);
#9747=PRODUCT_DEFINITION_FORMATION('',$,#9774);
#9748=PRODUCT_RELATED_PRODUCT_CATEGORY('MAS-611',
'MAS-611',(#9763));
#9749=PRODUCT_RELATED_PRODUCT_CATEGORY('VALVE_BODY','VALVE_BODY',(#9764));
#9750=PRODUCT_RELATED_PRODUCT_CATEGORY('VALVE_DISC','VALVE_DISC',(#9765));
#9751=PRODUCT_RELATED_PRODUCT_CATEGORY('SPINDLE','SPINDLE',(#9766));
#9752=PRODUCT_RELATED_PRODUCT_CATEGORY('SPINDLE_COLLAR',
'SPINDLE_COLLAR',(#9767));
#9753=PRODUCT_RELATED_PRODUCT_CATEGORY('RETAINING_PIN','RETAINING_PIN',
(#9768));
#9754=PRODUCT_RELATED_PRODUCT_CATEGORY('BONNET_COVER','BONNET_COVER',(#9769));
#9755=PRODUCT_RELATED_PRODUCT_CATEGORY('PACKING_GLAND','PACKING_GLAND',
(#9770));
#9756=PRODUCT_RELATED_PRODUCT_CATEGORY('GLAND_NUT','GLAND_NUT',(#9771));
#9757=PRODUCT_RELATED_PRODUCT_CATEGORY('HANDWHEEL','HANDWHEEL',(#9772));
#9758=PRODUCT_RELATED_PRODUCT_CATEGORY('NUT','NUT',(#9773));
#9759=PRODUCT_RELATED_PRODUCT_CATEGORY('BOLT','BOLT',(#9774));
#9760=APPLICATION_PROTOCOL_DEFINITION('international standard',
'automotive_design',2009,#9761);
#9761=APPLICATION_CONTEXT(
'Core Data for Automotive Mechanical Design Process');
#9762=PRODUCT_CONTEXT('part definition',#9761,'mechanical');
#9763=PRODUCT('2026-10-04-08-13-48-879','MAS-611',$,(#9762));
#9764=PRODUCT('2026-10-04-08-13-48-880','VALVE_BODY','PART',(#9762));
#9765=PRODUCT('2026-10-04-08-13-48-881','VALVE_DISC','PART',(#9762));
#9766=PRODUCT('2026-10-04-08-13-48-882','SPINDLE','PART',(#9762));
#9767=PRODUCT('2026-10-04-08-13-48-883','SPINDLE_COLLAR','PART',(#9762));
#9768=PRODUCT('2026-10-04-08-13-48-884','RETAINING_PIN','PART',(#9762));
#9769=PRODUCT('2026-10-04-08-13-48-885','BONNET_COVER','PART',(#9762));
#9770=PRODUCT('2026-10-04-08-13-48-886','PACKING_GLAND','PART',(#9762));
#9771=PRODUCT('2026-10-04-08-13-48-887','GLAND_NUT','PART',(#9762));
#9772=PRODUCT('2026-10-04-08-13-48-888','HANDWHEEL','PART',(#9762));
#9773=PRODUCT('2026-10-04-08-13-48-889','NUT','PART',(#9762));
#9774=PRODUCT('2026-10-04-08-13-48-890','BOLT','PART',(#9762));
#9775=PRESENTATION_STYLE_ASSIGNMENT((#9776));
#9776=SURFACE_STYLE_USAGE(.BOTH.,#9777);
#9777=SURFACE_SIDE_STYLE('',(#9778));
#9778=SURFACE_STYLE_FILL_AREA(#9779);
#9779=FILL_AREA_STYLE('Steel - Satin',(#9780));
#9780=FILL_AREA_STYLE_COLOUR('Steel - Satin',#9781);
#9781=COLOUR_RGB('Steel - Satin', 0.09019608, 0.27058824, 0.51372549);
ENDSEC;
END-ISO-10303-21;
